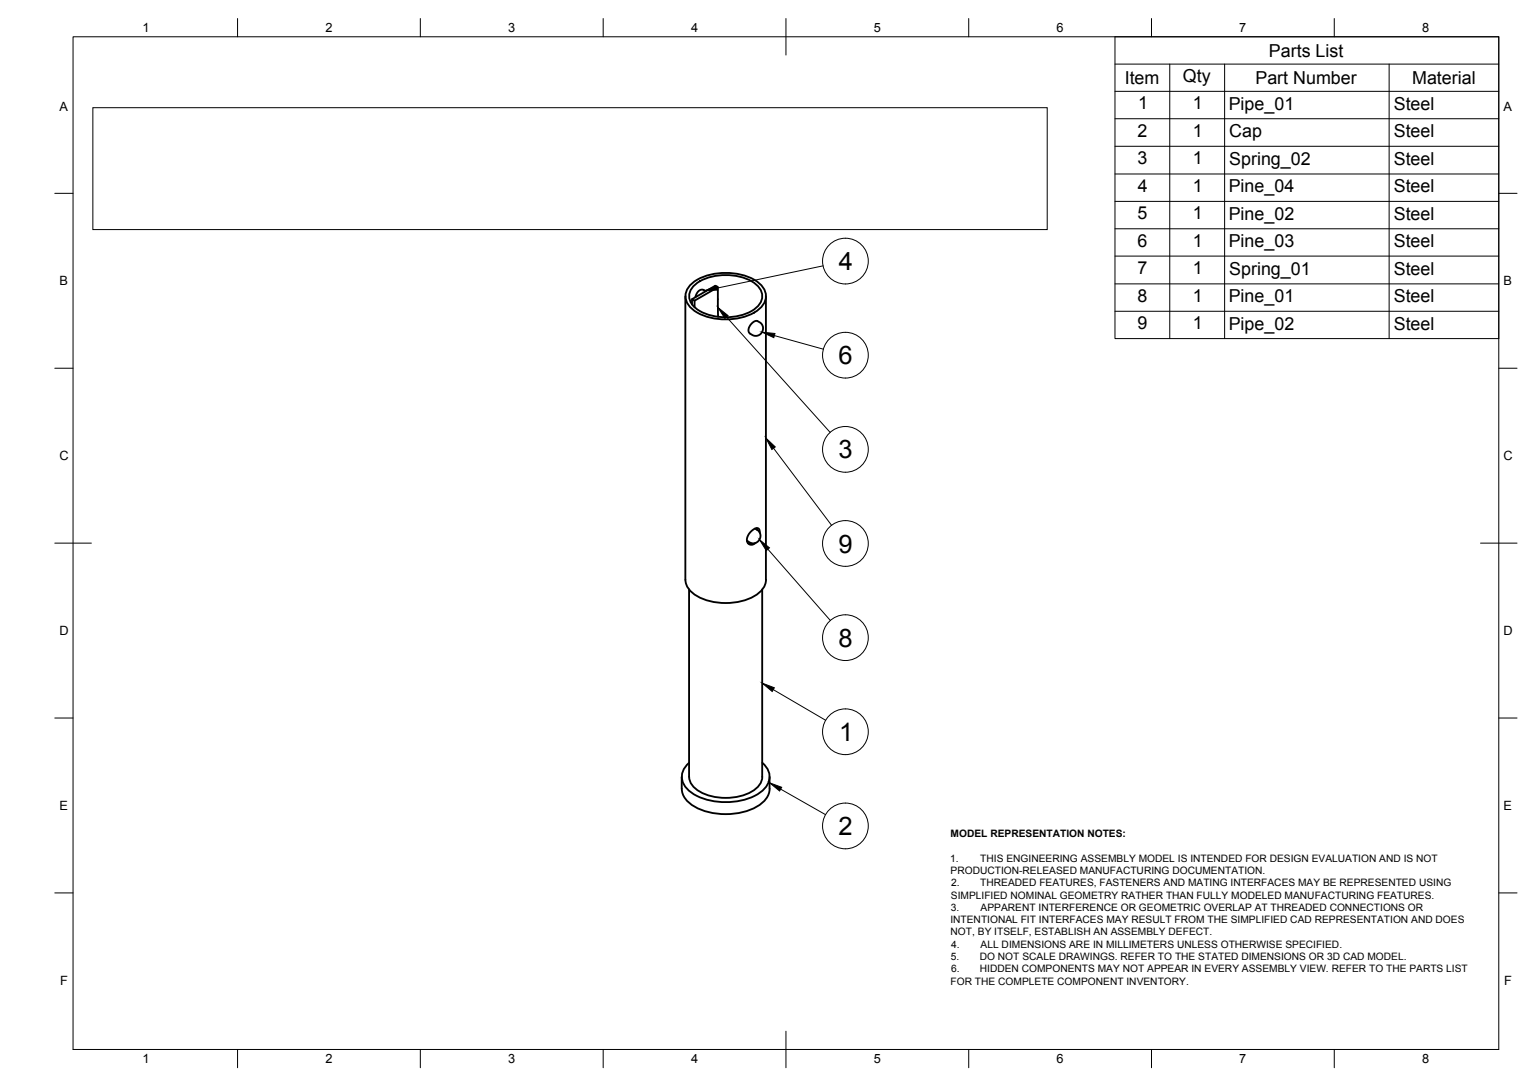
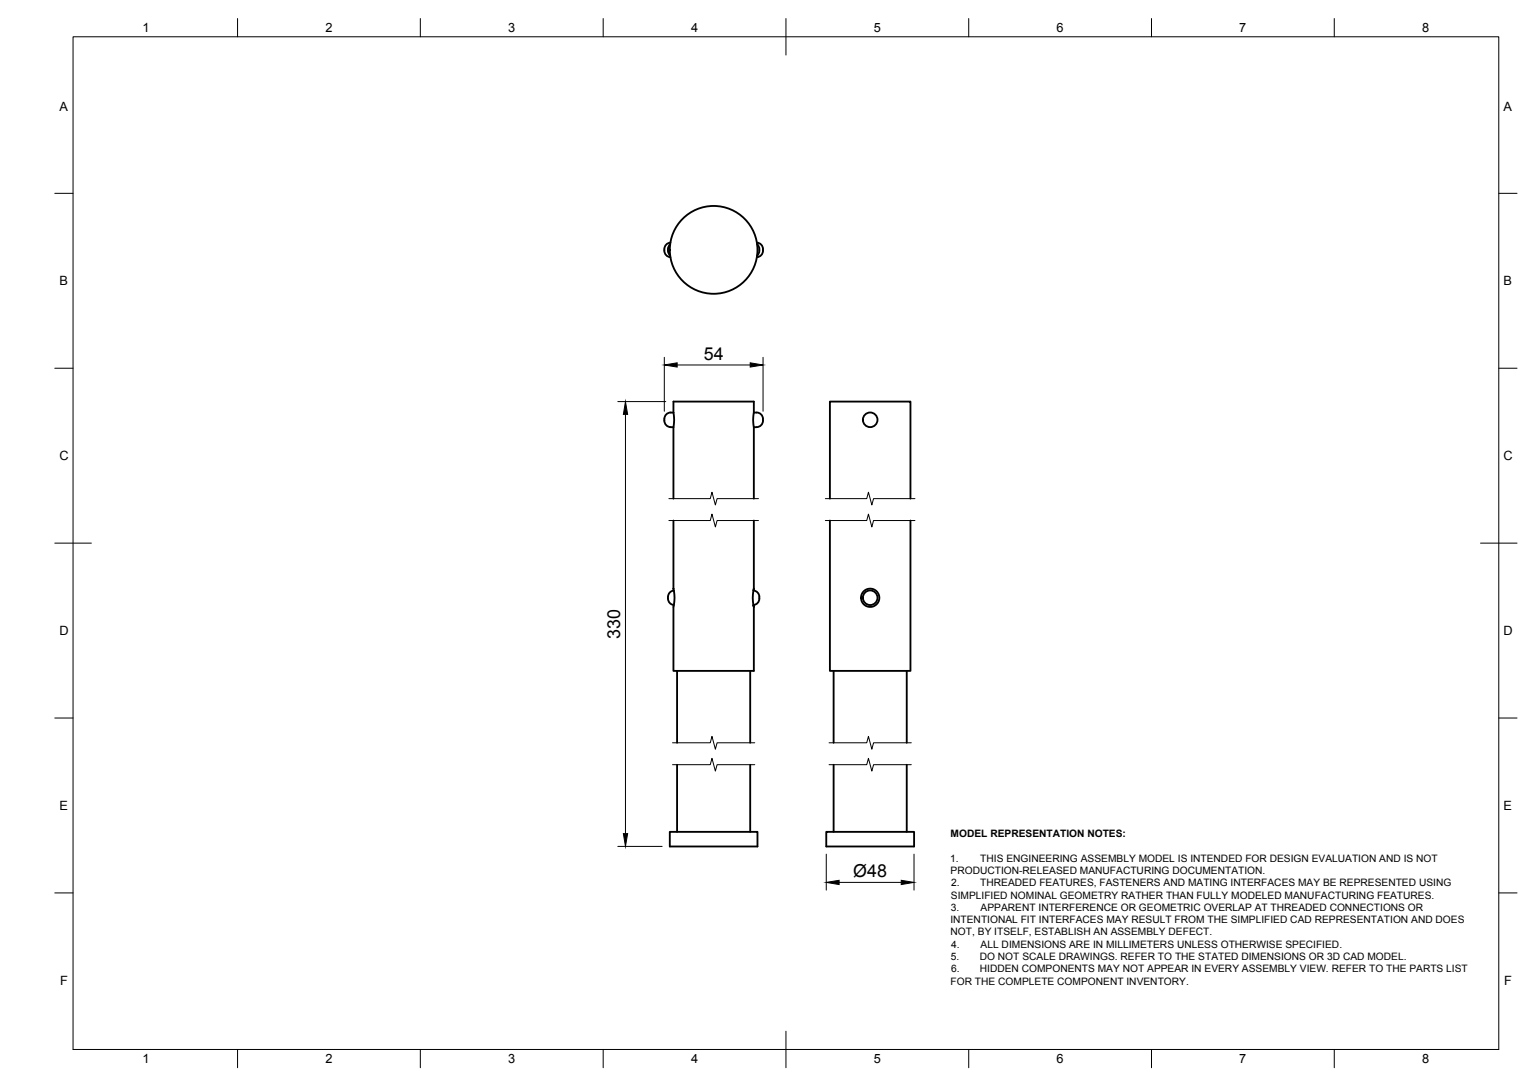
ISO-10303-21;
HEADER;
/* Generated by software containing ST-Developer
 * from STEP Tools, Inc. (www.steptools.com) 
 */

FILE_DESCRIPTION(
/* description */ (''),
/* implementation_level */ '2;1');

FILE_NAME(
/* name */ 'BR-354',
/* time_stamp */ '2026-10-06T13:31:15-07:00',
/* author */ (''),
/* organization */ (''),
/* preprocessor_version */ 'ST-DEVELOPER v20.2',
/* originating_system */ 'Autodesk Translation Framework v15.15.0.0',
/* authorisation */ '');

FILE_SCHEMA (('AUTOMOTIVE_DESIGN { 1 0 10303 214 3 1 1 }'));
ENDSEC;

DATA;
#10=MECHANICAL_DESIGN_GEOMETRIC_PRESENTATION_REPRESENTATION('',(#79,#80,
#81,#82,#83,#84,#85,#86,#87),#3154);
#11=ITEM_DEFINED_TRANSFORMATION($,$,#1191,#1277);
#12=ITEM_DEFINED_TRANSFORMATION($,$,#1202,#1278);
#13=ITEM_DEFINED_TRANSFORMATION($,$,#1212,#1279);
#14=ITEM_DEFINED_TRANSFORMATION($,$,#1221,#1280);
#15=ITEM_DEFINED_TRANSFORMATION($,$,#1230,#1281);
#16=ITEM_DEFINED_TRANSFORMATION($,$,#1239,#1282);
#17=ITEM_DEFINED_TRANSFORMATION($,$,#1248,#1283);
#18=ITEM_DEFINED_TRANSFORMATION($,$,#1257,#1284);
#19=ITEM_DEFINED_TRANSFORMATION($,$,#1266,#1285);
#20=(
REPRESENTATION_RELATIONSHIP($,$,#3189,#3188)
REPRESENTATION_RELATIONSHIP_WITH_TRANSFORMATION(#11)
SHAPE_REPRESENTATION_RELATIONSHIP()
);
#21=(
REPRESENTATION_RELATIONSHIP($,$,#3190,#3188)
REPRESENTATION_RELATIONSHIP_WITH_TRANSFORMATION(#12)
SHAPE_REPRESENTATION_RELATIONSHIP()
);
#22=(
REPRESENTATION_RELATIONSHIP($,$,#3191,#3188)
REPRESENTATION_RELATIONSHIP_WITH_TRANSFORMATION(#13)
SHAPE_REPRESENTATION_RELATIONSHIP()
);
#23=(
REPRESENTATION_RELATIONSHIP($,$,#3192,#3188)
REPRESENTATION_RELATIONSHIP_WITH_TRANSFORMATION(#14)
SHAPE_REPRESENTATION_RELATIONSHIP()
);
#24=(
REPRESENTATION_RELATIONSHIP($,$,#3193,#3188)
REPRESENTATION_RELATIONSHIP_WITH_TRANSFORMATION(#15)
SHAPE_REPRESENTATION_RELATIONSHIP()
);
#25=(
REPRESENTATION_RELATIONSHIP($,$,#3194,#3188)
REPRESENTATION_RELATIONSHIP_WITH_TRANSFORMATION(#16)
SHAPE_REPRESENTATION_RELATIONSHIP()
);
#26=(
REPRESENTATION_RELATIONSHIP($,$,#3195,#3188)
REPRESENTATION_RELATIONSHIP_WITH_TRANSFORMATION(#17)
SHAPE_REPRESENTATION_RELATIONSHIP()
);
#27=(
REPRESENTATION_RELATIONSHIP($,$,#3196,#3188)
REPRESENTATION_RELATIONSHIP_WITH_TRANSFORMATION(#18)
SHAPE_REPRESENTATION_RELATIONSHIP()
);
#28=(
REPRESENTATION_RELATIONSHIP($,$,#3197,#3188)
REPRESENTATION_RELATIONSHIP_WITH_TRANSFORMATION(#19)
SHAPE_REPRESENTATION_RELATIONSHIP()
);
#29=CONTEXT_DEPENDENT_SHAPE_REPRESENTATION(#20,#3179);
#30=CONTEXT_DEPENDENT_SHAPE_REPRESENTATION(#21,#3180);
#31=CONTEXT_DEPENDENT_SHAPE_REPRESENTATION(#22,#3181);
#32=CONTEXT_DEPENDENT_SHAPE_REPRESENTATION(#23,#3182);
#33=CONTEXT_DEPENDENT_SHAPE_REPRESENTATION(#24,#3183);
#34=CONTEXT_DEPENDENT_SHAPE_REPRESENTATION(#25,#3184);
#35=CONTEXT_DEPENDENT_SHAPE_REPRESENTATION(#26,#3185);
#36=CONTEXT_DEPENDENT_SHAPE_REPRESENTATION(#27,#3186);
#37=CONTEXT_DEPENDENT_SHAPE_REPRESENTATION(#28,#3187);
#38=NEXT_ASSEMBLY_USAGE_OCCURRENCE('Pipe_01:1','Pipe_01:1','Pipe_01:1',
#3199,#3200,'Pipe_01:1');
#39=NEXT_ASSEMBLY_USAGE_OCCURRENCE('Cap:1','Cap:1','Cap:1',#3199,#3201,
'Cap:1');
#40=NEXT_ASSEMBLY_USAGE_OCCURRENCE('Spring_02:1','Spring_02:1',
'Spring_02:1',#3199,#3202,'Spring_02:1');
#41=NEXT_ASSEMBLY_USAGE_OCCURRENCE('Pine_04:1','Pine_04:1','Pine_04:1',
#3199,#3203,'Pine_04:1');
#42=NEXT_ASSEMBLY_USAGE_OCCURRENCE('Pine_02:1','Pine_02:1','Pine_02:1',
#3199,#3204,'Pine_02:1');
#43=NEXT_ASSEMBLY_USAGE_OCCURRENCE('Pine_03:1','Pine_03:1','Pine_03:1',
#3199,#3205,'Pine_03:1');
#44=NEXT_ASSEMBLY_USAGE_OCCURRENCE('Spring_01:1','Spring_01:1',
'Spring_01:1',#3199,#3206,'Spring_01:1');
#45=NEXT_ASSEMBLY_USAGE_OCCURRENCE('Pine_01:1','Pine_01:1','Pine_01:1',
#3199,#3207,'Pine_01:1');
#46=NEXT_ASSEMBLY_USAGE_OCCURRENCE('Pipe_02:1','Pipe_02:1','Pipe_02:1',
#3199,#3208,'Pipe_02:1');
#47=(
BOUNDED_SURFACE()
B_SPLINE_SURFACE(2,2,((#2142,#2143,#2144,#2145,#2146,#2147,#2148,#2149,
#2150),(#2151,#2152,#2153,#2154,#2155,#2156,#2157,#2158,#2159),(#2160,#2161,
#2162,#2163,#2164,#2165,#2166,#2167,#2168)),.UNSPECIFIED.,.F.,.T.,.F.)
B_SPLINE_SURFACE_WITH_KNOTS((3,3),(3,2,2,2,3),(-1.57079632679497,6.11109985317371E-14),
(-3.14159265358979,-1.5707963267949,0.,1.5707963267949,3.14159265358979),
 .UNSPECIFIED.)
GEOMETRIC_REPRESENTATION_ITEM()
RATIONAL_B_SPLINE_SURFACE(((1.,0.707106781186548,1.,0.707106781186548,1.,
0.707106781186548,1.,0.707106781186548,1.),(0.707106781186505,0.49999999999997,
0.707106781186505,0.49999999999997,0.707106781186505,0.49999999999997,0.707106781186505,
0.49999999999997,0.707106781186505),(1.,0.707106781186548,1.,0.707106781186548,
1.,0.707106781186548,1.,0.707106781186548,1.)))
REPRESENTATION_ITEM('')
SURFACE()
);
#48=(
BOUNDED_SURFACE()
B_SPLINE_SURFACE(2,2,((#2183,#2184,#2185,#2186,#2187,#2188,#2189,#2190,
#2191),(#2192,#2193,#2194,#2195,#2196,#2197,#2198,#2199,#2200),(#2201,#2202,
#2203,#2204,#2205,#2206,#2207,#2208,#2209)),.UNSPECIFIED.,.F.,.T.,.F.)
B_SPLINE_SURFACE_WITH_KNOTS((3,3),(3,2,2,2,3),(-1.57079632679509,1.96675441490332E-13),
(-3.14159265358979,-1.5707963267949,0.,1.5707963267949,3.14159265358979),
 .UNSPECIFIED.)
GEOMETRIC_REPRESENTATION_ITEM()
RATIONAL_B_SPLINE_SURFACE(((1.,0.707106781186548,1.,0.707106781186548,1.,
0.707106781186548,1.,0.707106781186548,1.),(0.707106781186405,0.499999999999899,
0.707106781186405,0.499999999999899,0.707106781186405,0.499999999999899,
0.707106781186405,0.499999999999899,0.707106781186405),(1.,0.707106781186548,
1.,0.707106781186548,1.,0.707106781186548,1.,0.707106781186548,1.)))
REPRESENTATION_ITEM('')
SURFACE()
);
#49=(
BOUNDED_SURFACE()
B_SPLINE_SURFACE(2,2,((#2224,#2225,#2226,#2227,#2228,#2229,#2230,#2231,
#2232),(#2233,#2234,#2235,#2236,#2237,#2238,#2239,#2240,#2241),(#2242,#2243,
#2244,#2245,#2246,#2247,#2248,#2249,#2250)),.UNSPECIFIED.,.F.,.T.,.F.)
B_SPLINE_SURFACE_WITH_KNOTS((3,3),(3,2,2,2,3),(-6.11109985317371E-14,1.57079632679497),
(-3.14159265358979,-1.5707963267949,0.,1.5707963267949,3.14159265358979),
 .UNSPECIFIED.)
GEOMETRIC_REPRESENTATION_ITEM()
RATIONAL_B_SPLINE_SURFACE(((1.,0.707106781186548,1.,0.707106781186548,1.,
0.707106781186548,1.,0.707106781186548,1.),(0.707106781186505,0.49999999999997,
0.707106781186505,0.49999999999997,0.707106781186505,0.49999999999997,0.707106781186505,
0.49999999999997,0.707106781186505),(1.,0.707106781186548,1.,0.707106781186548,
1.,0.707106781186548,1.,0.707106781186548,1.)))
REPRESENTATION_ITEM('')
SURFACE()
);
#50=(
BOUNDED_SURFACE()
B_SPLINE_SURFACE(2,2,((#2568,#2569,#2570,#2571,#2572,#2573,#2574,#2575,
#2576),(#2577,#2578,#2579,#2580,#2581,#2582,#2583,#2584,#2585),(#2586,#2587,
#2588,#2589,#2590,#2591,#2592,#2593,#2594)),.UNSPECIFIED.,.F.,.T.,.F.)
B_SPLINE_SURFACE_WITH_KNOTS((3,3),(3,2,2,2,3),(-1.96675441490332E-13,1.57079632679509),
(-3.14159265358979,-1.5707963267949,0.,1.5707963267949,3.14159265358979),
 .UNSPECIFIED.)
GEOMETRIC_REPRESENTATION_ITEM()
RATIONAL_B_SPLINE_SURFACE(((1.,0.707106781186548,1.,0.707106781186548,1.,
0.707106781186548,1.,0.707106781186548,1.),(0.707106781186405,0.499999999999899,
0.707106781186405,0.499999999999899,0.707106781186405,0.499999999999899,
0.707106781186405,0.499999999999899,0.707106781186405),(1.,0.707106781186548,
1.,0.707106781186548,1.,0.707106781186548,1.,0.707106781186548,1.)))
REPRESENTATION_ITEM('')
SURFACE()
);
#51=B_SPLINE_SURFACE_WITH_KNOTS('',3,1,((#1764,#1765),(#1766,#1767),(#1768,
#1769),(#1770,#1771),(#1772,#1773),(#1774,#1775),(#1776,#1777),(#1778,#1779),
(#1780,#1781),(#1782,#1783),(#1784,#1785),(#1786,#1787),(#1788,#1789),(#1790,
#1791),(#1792,#1793),(#1794,#1795),(#1796,#1797),(#1798,#1799),(#1800,#1801)),
 .UNSPECIFIED.,.F.,.F.,.F.,(4,3,3,3,3,3,4),(2,2),(0.,0.25,0.625,0.869068416619454,
0.996324238316631,1.,1.10633190132162),(0.,2.16230058202055),
 .UNSPECIFIED.);
#52=B_SPLINE_SURFACE_WITH_KNOTS('',5,1,((#1843,#1844),(#1845,#1846),(#1847,
#1848),(#1849,#1850),(#1851,#1852),(#1853,#1854),(#1855,#1856),(#1857,#1858),
(#1859,#1860),(#1861,#1862),(#1863,#1864),(#1865,#1866),(#1867,#1868),(#1869,
#1870),(#1871,#1872),(#1873,#1874),(#1875,#1876),(#1877,#1878),(#1879,#1880),
(#1881,#1882),(#1883,#1884),(#1885,#1886),(#1887,#1888),(#1889,#1890),(#1891,
#1892)),.UNSPECIFIED.,.F.,.F.,.F.,(6,5,1,1,1,1,1,1,1,1,1,1,1,1,1,1,6),(2,
2),(-1.10044937423827,-1.,-0.933333333333333,-0.866666666666667,-0.8,-0.733333333333333,
-0.666666666666667,-0.6,-0.533333333333333,-0.466666666666667,-0.4,-0.333333333333333,
-0.266666666666667,-0.2,-0.133333333333333,-0.0666666666666667,0.),(0.,
2.16),.UNSPECIFIED.);
#53=B_SPLINE_SURFACE_WITH_KNOTS('',5,1,((#2046,#2047),(#2048,#2049),(#2050,
#2051),(#2052,#2053),(#2054,#2055),(#2056,#2057),(#2058,#2059),(#2060,#2061),
(#2062,#2063),(#2064,#2065),(#2066,#2067),(#2068,#2069),(#2070,#2071),(#2072,
#2073),(#2074,#2075),(#2076,#2077),(#2078,#2079),(#2080,#2081),(#2082,#2083),
(#2084,#2085),(#2086,#2087),(#2088,#2089),(#2090,#2091),(#2092,#2093),(#2094,
#2095)),.UNSPECIFIED.,.F.,.F.,.F.,(6,1,1,1,1,1,1,1,1,1,1,1,1,1,1,5,6),(2,
2),(0.,0.0666666666666667,0.133333333333333,0.2,0.266666666666667,0.333333333333333,
0.4,0.466666666666667,0.533333333333333,0.6,0.666666666666667,0.733333333333333,
0.8,0.866666666666667,0.933333333333333,1.,1.10044937423827),(0.,2.16),
 .UNSPECIFIED.);
#54=B_SPLINE_SURFACE_WITH_KNOTS('',3,1,((#2103,#2104),(#2105,#2106),(#2107,
#2108),(#2109,#2110),(#2111,#2112),(#2113,#2114),(#2115,#2116),(#2117,#2118),
(#2119,#2120),(#2121,#2122),(#2123,#2124),(#2125,#2126),(#2127,#2128),(#2129,
#2130),(#2131,#2132),(#2133,#2134),(#2135,#2136),(#2137,#2138),(#2139,#2140)),
 .UNSPECIFIED.,.F.,.F.,.F.,(4,3,3,3,3,3,4),(2,2),(-1.10633190132173,-1.,
-0.996324238316733,-0.869068416619454,-0.625,-0.25,0.),(0.,2.16230058202055),
 .UNSPECIFIED.);
#55=B_SPLINE_SURFACE_WITH_KNOTS('',5,1,((#2342,#2343),(#2344,#2345),(#2346,
#2347),(#2348,#2349),(#2350,#2351),(#2352,#2353),(#2354,#2355),(#2356,#2357),
(#2358,#2359),(#2360,#2361),(#2362,#2363),(#2364,#2365),(#2366,#2367),(#2368,
#2369),(#2370,#2371),(#2372,#2373),(#2374,#2375),(#2376,#2377),(#2378,#2379),
(#2380,#2381)),.UNSPECIFIED.,.F.,.F.,.F.,(6,1,1,1,1,1,1,1,1,1,1,1,1,1,1,
6),(2,2),(-1.,-0.933333333333333,-0.866666666666667,-0.8,-0.733333333333333,
-0.666666666666667,-0.6,-0.533333333333333,-0.466666666666667,-0.4,-0.333333333333333,
-0.266666666666667,-0.2,-0.133333333333333,-0.0666666666666667,0.),(0.,
2.16),.UNSPECIFIED.);
#56=B_SPLINE_SURFACE_WITH_KNOTS('',5,1,((#2406,#2407),(#2408,#2409),(#2410,
#2411),(#2412,#2413),(#2414,#2415),(#2416,#2417),(#2418,#2419),(#2420,#2421),
(#2422,#2423),(#2424,#2425),(#2426,#2427),(#2428,#2429),(#2430,#2431),(#2432,
#2433),(#2434,#2435),(#2436,#2437),(#2438,#2439),(#2440,#2441),(#2442,#2443),
(#2444,#2445)),.UNSPECIFIED.,.F.,.F.,.F.,(6,1,1,1,1,1,1,1,1,1,1,1,1,1,1,
6),(2,2),(0.,0.0666666666666667,0.133333333333333,0.2,0.266666666666667,
0.333333333333333,0.4,0.466666666666667,0.533333333333333,0.6,0.666666666666667,
0.733333333333333,0.8,0.866666666666667,0.933333333333333,1.),(0.,2.16),
 .UNSPECIFIED.);
#57=B_SPLINE_SURFACE_WITH_KNOTS('',3,1,((#2480,#2481),(#2482,#2483),(#2484,
#2485),(#2486,#2487),(#2488,#2489),(#2490,#2491),(#2492,#2493),(#2494,#2495),
(#2496,#2497),(#2498,#2499),(#2500,#2501),(#2502,#2503),(#2504,#2505)),
 .UNSPECIFIED.,.F.,.F.,.F.,(4,3,3,3,4),(2,2),(-0.996324238316733,-0.869068416619454,
-0.625,-0.25,0.),(0.,2.16230058202055),.UNSPECIFIED.);
#58=B_SPLINE_SURFACE_WITH_KNOTS('',3,1,((#2518,#2519),(#2520,#2521),(#2522,
#2523),(#2524,#2525),(#2526,#2527),(#2528,#2529),(#2530,#2531),(#2532,#2533),
(#2534,#2535),(#2536,#2537),(#2538,#2539),(#2540,#2541),(#2542,#2543)),
 .UNSPECIFIED.,.F.,.F.,.F.,(4,3,3,3,4),(2,2),(0.,0.25,0.625,0.869068416619454,
0.996324238316631),(0.,2.16230058202055),.UNSPECIFIED.);
#59=B_SPLINE_SURFACE_WITH_KNOTS('',3,1,((#2777,#2778),(#2779,#2780),(#2781,
#2782),(#2783,#2784),(#2785,#2786),(#2787,#2788),(#2789,#2790),(#2791,#2792),
(#2793,#2794),(#2795,#2796),(#2797,#2798),(#2799,#2800),(#2801,#2802),(#2803,
#2804),(#2805,#2806),(#2807,#2808),(#2809,#2810),(#2811,#2812),(#2813,#2814),
(#2815,#2816),(#2817,#2818),(#2819,#2820),(#2821,#2822),(#2823,#2824),(#2825,
#2826),(#2827,#2828),(#2829,#2830),(#2831,#2832),(#2833,#2834),(#2835,#2836),
(#2837,#2838),(#2839,#2840),(#2841,#2842),(#2843,#2844),(#2845,#2846),(#2847,
#2848),(#2849,#2850)),.UNSPECIFIED.,.T.,.F.,.F.,(4,3,3,3,3,3,3,3,3,3,3,
3,4),(2,2),(-2.41782189489405,-2.24947880033894,-1.98878599548315,-1.8058107663078,
-1.62285095130575,-1.4611068129162,-1.2281083508595,-1.04723806876992,-0.775359720885815,
-0.597430394095587,-0.415845402852008,-0.241029560217643,0.),(0.,28.8022414300165),
 .UNSPECIFIED.);
#60=B_SPLINE_SURFACE_WITH_KNOTS('',3,1,((#2932,#2933),(#2934,#2935),(#2936,
#2937),(#2938,#2939),(#2940,#2941),(#2942,#2943),(#2944,#2945),(#2946,#2947),
(#2948,#2949),(#2950,#2951),(#2952,#2953),(#2954,#2955),(#2956,#2957),(#2958,
#2959),(#2960,#2961),(#2962,#2963),(#2964,#2965),(#2966,#2967),(#2968,#2969),
(#2970,#2971),(#2972,#2973),(#2974,#2975),(#2976,#2977),(#2978,#2979),(#2980,
#2981),(#2982,#2983),(#2984,#2985),(#2986,#2987),(#2988,#2989),(#2990,#2991),
(#2992,#2993),(#2994,#2995),(#2996,#2997),(#2998,#2999),(#3000,#3001),(#3002,
#3003),(#3004,#3005)),.UNSPECIFIED.,.T.,.F.,.F.,(4,3,3,3,3,3,3,3,3,3,3,
3,4),(2,2),(-2.41782189489405,-2.24947880033894,-1.98878599548315,-1.8058107663078,
-1.62285095130575,-1.4611068129162,-1.2281083508595,-1.04723806876992,-0.775359720885815,
-0.597430394095587,-0.415845402852008,-0.241029560217643,0.),(0.,28.8022414300165),
 .UNSPECIFIED.);
#61=SHAPE_REPRESENTATION_RELATIONSHIP('SRR','None',#3189,#70);
#62=SHAPE_REPRESENTATION_RELATIONSHIP('SRR','None',#3190,#71);
#63=SHAPE_REPRESENTATION_RELATIONSHIP('SRR','None',#3191,#72);
#64=SHAPE_REPRESENTATION_RELATIONSHIP('SRR','None',#3192,#73);
#65=SHAPE_REPRESENTATION_RELATIONSHIP('SRR','None',#3193,#74);
#66=SHAPE_REPRESENTATION_RELATIONSHIP('SRR','None',#3194,#75);
#67=SHAPE_REPRESENTATION_RELATIONSHIP('SRR','None',#3195,#76);
#68=SHAPE_REPRESENTATION_RELATIONSHIP('SRR','None',#3196,#77);
#69=SHAPE_REPRESENTATION_RELATIONSHIP('SRR','None',#3197,#78);
#70=ADVANCED_BREP_SHAPE_REPRESENTATION('',(#88),#3145);
#71=ADVANCED_BREP_SHAPE_REPRESENTATION('',(#89),#3146);
#72=ADVANCED_BREP_SHAPE_REPRESENTATION('',(#90),#3147);
#73=ADVANCED_BREP_SHAPE_REPRESENTATION('',(#91),#3148);
#74=ADVANCED_BREP_SHAPE_REPRESENTATION('',(#92),#3149);
#75=ADVANCED_BREP_SHAPE_REPRESENTATION('',(#93),#3150);
#76=ADVANCED_BREP_SHAPE_REPRESENTATION('',(#94),#3151);
#77=ADVANCED_BREP_SHAPE_REPRESENTATION('',(#95),#3152);
#78=ADVANCED_BREP_SHAPE_REPRESENTATION('',(#96),#3153);
#79=STYLED_ITEM('',(#3243),#88);
#80=STYLED_ITEM('',(#3243),#89);
#81=STYLED_ITEM('',(#3243),#90);
#82=STYLED_ITEM('',(#3243),#91);
#83=STYLED_ITEM('',(#3243),#92);
#84=STYLED_ITEM('',(#3243),#93);
#85=STYLED_ITEM('',(#3243),#94);
#86=STYLED_ITEM('',(#3243),#95);
#87=STYLED_ITEM('',(#3243),#96);
#88=MANIFOLD_SOLID_BREP('Body1',#1081);
#89=MANIFOLD_SOLID_BREP('Body1',#1082);
#90=MANIFOLD_SOLID_BREP('Body1',#1083);
#91=MANIFOLD_SOLID_BREP('Body1',#1084);
#92=MANIFOLD_SOLID_BREP('Body1',#1085);
#93=MANIFOLD_SOLID_BREP('Body1',#1086);
#94=MANIFOLD_SOLID_BREP('Body1',#1087);
#95=MANIFOLD_SOLID_BREP('Body1',#1088);
#96=MANIFOLD_SOLID_BREP('Body1',#1089);
#97=PLANE('',#1200);
#98=PLANE('',#1201);
#99=PLANE('',#1203);
#100=PLANE('',#1210);
#101=PLANE('',#1211);
#102=PLANE('',#1213);
#103=PLANE('',#1214);
#104=PLANE('',#1215);
#105=PLANE('',#1216);
#106=PLANE('',#1217);
#107=PLANE('',#1218);
#108=PLANE('',#1219);
#109=PLANE('',#1220);
#110=PLANE('',#1228);
#111=PLANE('',#1229);
#112=PLANE('',#1237);
#113=PLANE('',#1238);
#114=PLANE('',#1246);
#115=PLANE('',#1247);
#116=PLANE('',#1249);
#117=PLANE('',#1250);
#118=PLANE('',#1251);
#119=PLANE('',#1252);
#120=PLANE('',#1253);
#121=PLANE('',#1254);
#122=PLANE('',#1255);
#123=PLANE('',#1256);
#124=PLANE('',#1264);
#125=PLANE('',#1265);
#126=PLANE('',#1269);
#127=PLANE('',#1276);
#128=FACE_BOUND('',#233,.T.);
#129=FACE_BOUND('',#235,.T.);
#130=FACE_BOUND('',#237,.T.);
#131=FACE_BOUND('',#239,.T.);
#132=FACE_BOUND('',#245,.T.);
#133=FACE_BOUND('',#291,.T.);
#134=FACE_BOUND('',#293,.T.);
#135=FACE_BOUND('',#294,.T.);
#136=FACE_BOUND('',#296,.T.);
#137=FACE_BOUND('',#297,.T.);
#138=FACE_BOUND('',#299,.T.);
#139=CIRCLE('',#1195,18.);
#140=CIRCLE('',#1196,18.);
#141=CIRCLE('',#1198,20.);
#142=CIRCLE('',#1199,20.);
#143=CIRCLE('',#1204,20.);
#144=CIRCLE('',#1206,20.);
#145=CIRCLE('',#1208,24.);
#146=CIRCLE('',#1209,24.);
#147=CIRCLE('',#1222,3.99999999999999);
#148=CIRCLE('',#1223,3.99999999999999);
#149=CIRCLE('',#1224,3.49999999999999);
#150=CIRCLE('',#1225,0.49999999999999);
#151=CIRCLE('',#1227,3.99999999999999);
#152=CIRCLE('',#1231,3.99999999999999);
#153=CIRCLE('',#1232,3.99999999999999);
#154=CIRCLE('',#1233,3.49999999999994);
#155=CIRCLE('',#1234,0.49999999999999);
#156=CIRCLE('',#1236,3.99999999999999);
#157=CIRCLE('',#1240,3.99999999999999);
#158=CIRCLE('',#1241,3.49999999999999);
#159=CIRCLE('',#1242,0.49999999999999);
#160=CIRCLE('',#1243,3.99999999999999);
#161=CIRCLE('',#1245,3.99999999999999);
#162=CIRCLE('',#1258,3.99999999999999);
#163=CIRCLE('',#1259,3.49999999999994);
#164=CIRCLE('',#1260,0.49999999999999);
#165=CIRCLE('',#1261,3.99999999999999);
#166=CIRCLE('',#1263,3.99999999999999);
#167=CIRCLE('',#1270,22.);
#168=CIRCLE('',#1271,20.);
#169=CIRCLE('',#1273,20.);
#170=CIRCLE('',#1275,22.);
#171=FACE_OUTER_BOUND('',#230,.T.);
#172=FACE_OUTER_BOUND('',#231,.T.);
#173=FACE_OUTER_BOUND('',#232,.T.);
#174=FACE_OUTER_BOUND('',#234,.T.);
#175=FACE_OUTER_BOUND('',#236,.T.);
#176=FACE_OUTER_BOUND('',#238,.T.);
#177=FACE_OUTER_BOUND('',#240,.T.);
#178=FACE_OUTER_BOUND('',#241,.T.);
#179=FACE_OUTER_BOUND('',#242,.T.);
#180=FACE_OUTER_BOUND('',#243,.T.);
#181=FACE_OUTER_BOUND('',#244,.T.);
#182=FACE_OUTER_BOUND('',#246,.T.);
#183=FACE_OUTER_BOUND('',#247,.T.);
#184=FACE_OUTER_BOUND('',#248,.T.);
#185=FACE_OUTER_BOUND('',#249,.T.);
#186=FACE_OUTER_BOUND('',#250,.T.);
#187=FACE_OUTER_BOUND('',#251,.T.);
#188=FACE_OUTER_BOUND('',#252,.T.);
#189=FACE_OUTER_BOUND('',#253,.T.);
#190=FACE_OUTER_BOUND('',#254,.T.);
#191=FACE_OUTER_BOUND('',#255,.T.);
#192=FACE_OUTER_BOUND('',#256,.T.);
#193=FACE_OUTER_BOUND('',#257,.T.);
#194=FACE_OUTER_BOUND('',#258,.T.);
#195=FACE_OUTER_BOUND('',#259,.T.);
#196=FACE_OUTER_BOUND('',#260,.T.);
#197=FACE_OUTER_BOUND('',#261,.T.);
#198=FACE_OUTER_BOUND('',#262,.T.);
#199=FACE_OUTER_BOUND('',#263,.T.);
#200=FACE_OUTER_BOUND('',#264,.T.);
#201=FACE_OUTER_BOUND('',#265,.T.);
#202=FACE_OUTER_BOUND('',#266,.T.);
#203=FACE_OUTER_BOUND('',#267,.T.);
#204=FACE_OUTER_BOUND('',#268,.T.);
#205=FACE_OUTER_BOUND('',#269,.T.);
#206=FACE_OUTER_BOUND('',#270,.T.);
#207=FACE_OUTER_BOUND('',#271,.T.);
#208=FACE_OUTER_BOUND('',#272,.T.);
#209=FACE_OUTER_BOUND('',#273,.T.);
#210=FACE_OUTER_BOUND('',#274,.T.);
#211=FACE_OUTER_BOUND('',#275,.T.);
#212=FACE_OUTER_BOUND('',#276,.T.);
#213=FACE_OUTER_BOUND('',#277,.T.);
#214=FACE_OUTER_BOUND('',#278,.T.);
#215=FACE_OUTER_BOUND('',#279,.T.);
#216=FACE_OUTER_BOUND('',#280,.T.);
#217=FACE_OUTER_BOUND('',#281,.T.);
#218=FACE_OUTER_BOUND('',#282,.T.);
#219=FACE_OUTER_BOUND('',#283,.T.);
#220=FACE_OUTER_BOUND('',#284,.T.);
#221=FACE_OUTER_BOUND('',#285,.T.);
#222=FACE_OUTER_BOUND('',#286,.T.);
#223=FACE_OUTER_BOUND('',#287,.T.);
#224=FACE_OUTER_BOUND('',#288,.T.);
#225=FACE_OUTER_BOUND('',#289,.T.);
#226=FACE_OUTER_BOUND('',#290,.T.);
#227=FACE_OUTER_BOUND('',#292,.T.);
#228=FACE_OUTER_BOUND('',#295,.T.);
#229=FACE_OUTER_BOUND('',#298,.T.);
#230=EDGE_LOOP('',(#720,#721,#722,#723,#724,#725,#726,#727));
#231=EDGE_LOOP('',(#728,#729,#730,#731,#732,#733));
#232=EDGE_LOOP('',(#734,#735,#736,#737,#738,#739,#740,#741,#742));
#233=EDGE_LOOP('',(#743,#744));
#234=EDGE_LOOP('',(#745,#746,#747,#748,#749,#750,#751,#752,#753));
#235=EDGE_LOOP('',(#754,#755));
#236=EDGE_LOOP('',(#756));
#237=EDGE_LOOP('',(#757));
#238=EDGE_LOOP('',(#758));
#239=EDGE_LOOP('',(#759));
#240=EDGE_LOOP('',(#760));
#241=EDGE_LOOP('',(#761,#762,#763,#764));
#242=EDGE_LOOP('',(#765,#766,#767,#768));
#243=EDGE_LOOP('',(#769));
#244=EDGE_LOOP('',(#770));
#245=EDGE_LOOP('',(#771));
#246=EDGE_LOOP('',(#772,#773,#774,#775));
#247=EDGE_LOOP('',(#776,#777,#778,#779));
#248=EDGE_LOOP('',(#780,#781,#782,#783));
#249=EDGE_LOOP('',(#784,#785,#786,#787));
#250=EDGE_LOOP('',(#788,#789,#790,#791));
#251=EDGE_LOOP('',(#792,#793,#794,#795,#796,#797,#798,#799,#800,#801));
#252=EDGE_LOOP('',(#802,#803,#804,#805,#806,#807,#808,#809,#810,#811));
#253=EDGE_LOOP('',(#812,#813,#814,#815));
#254=EDGE_LOOP('',(#816,#817,#818,#819));
#255=EDGE_LOOP('',(#820,#821,#822,#823));
#256=EDGE_LOOP('',(#824,#825,#826,#827));
#257=EDGE_LOOP('',(#828,#829,#830,#831));
#258=EDGE_LOOP('',(#832,#833,#834,#835,#836));
#259=EDGE_LOOP('',(#837,#838,#839,#840,#841));
#260=EDGE_LOOP('',(#842));
#261=EDGE_LOOP('',(#843));
#262=EDGE_LOOP('',(#844,#845,#846,#847,#848));
#263=EDGE_LOOP('',(#849,#850,#851,#852,#853));
#264=EDGE_LOOP('',(#854));
#265=EDGE_LOOP('',(#855));
#266=EDGE_LOOP('',(#856,#857,#858,#859,#860));
#267=EDGE_LOOP('',(#861,#862,#863,#864,#865));
#268=EDGE_LOOP('',(#866));
#269=EDGE_LOOP('',(#867));
#270=EDGE_LOOP('',(#868,#869,#870,#871,#872,#873,#874,#875,#876,#877));
#271=EDGE_LOOP('',(#878,#879,#880,#881));
#272=EDGE_LOOP('',(#882,#883,#884,#885));
#273=EDGE_LOOP('',(#886,#887,#888,#889));
#274=EDGE_LOOP('',(#890,#891,#892,#893));
#275=EDGE_LOOP('',(#894,#895,#896,#897));
#276=EDGE_LOOP('',(#898,#899,#900,#901));
#277=EDGE_LOOP('',(#902,#903,#904,#905));
#278=EDGE_LOOP('',(#906,#907,#908,#909));
#279=EDGE_LOOP('',(#910,#911,#912,#913));
#280=EDGE_LOOP('',(#914,#915,#916,#917));
#281=EDGE_LOOP('',(#918,#919,#920,#921,#922,#923,#924,#925,#926,#927));
#282=EDGE_LOOP('',(#928,#929,#930,#931,#932));
#283=EDGE_LOOP('',(#933,#934,#935,#936,#937));
#284=EDGE_LOOP('',(#938));
#285=EDGE_LOOP('',(#939));
#286=EDGE_LOOP('',(#940,#941,#942,#943,#944,#945));
#287=EDGE_LOOP('',(#946,#947,#948,#949,#950,#951,#952,#953,#954,#955));
#288=EDGE_LOOP('',(#956,#957,#958,#959));
#289=EDGE_LOOP('',(#960,#961,#962,#963,#964,#965,#966,#967));
#290=EDGE_LOOP('',(#968));
#291=EDGE_LOOP('',(#969));
#292=EDGE_LOOP('',(#970,#971,#972,#973,#974,#975,#976,#977,#978,#979,#980,
#981,#982,#983,#984));
#293=EDGE_LOOP('',(#985,#986));
#294=EDGE_LOOP('',(#987));
#295=EDGE_LOOP('',(#988,#989,#990,#991,#992,#993,#994,#995,#996,#997,#998,
#999,#1000,#1001,#1002));
#296=EDGE_LOOP('',(#1003,#1004));
#297=EDGE_LOOP('',(#1005));
#298=EDGE_LOOP('',(#1006));
#299=EDGE_LOOP('',(#1007));
#300=LINE('',#1580,#366);
#301=LINE('',#1672,#367);
#302=LINE('',#1713,#368);
#303=LINE('',#1715,#369);
#304=LINE('',#1720,#370);
#305=LINE('',#1722,#371);
#306=LINE('',#1732,#372);
#307=LINE('',#1738,#373);
#308=LINE('',#1746,#374);
#309=LINE('',#1748,#375);
#310=LINE('',#1750,#376);
#311=LINE('',#1751,#377);
#312=LINE('',#1755,#378);
#313=LINE('',#1756,#379);
#314=LINE('',#1757,#380);
#315=LINE('',#1761,#381);
#316=LINE('',#1762,#382);
#317=LINE('',#1763,#383);
#318=LINE('',#1804,#384);
#319=LINE('',#1919,#385);
#320=LINE('',#1966,#386);
#321=LINE('',#1968,#387);
#322=LINE('',#1970,#388);
#323=LINE('',#2022,#389);
#324=LINE('',#2024,#390);
#325=LINE('',#2026,#391);
#326=LINE('',#2096,#392);
#327=LINE('',#2098,#393);
#328=LINE('',#2100,#394);
#329=LINE('',#2102,#395);
#330=LINE('',#2179,#396);
#331=LINE('',#2220,#397);
#332=LINE('',#2260,#398);
#333=LINE('',#2268,#399);
#334=LINE('',#2312,#400);
#335=LINE('',#2314,#401);
#336=LINE('',#2316,#402);
#337=LINE('',#2340,#403);
#338=LINE('',#2341,#404);
#339=LINE('',#2383,#405);
#340=LINE('',#2405,#406);
#341=LINE('',#2467,#407);
#342=LINE('',#2470,#408);
#343=LINE('',#2471,#409);
#344=LINE('',#2474,#410);
#345=LINE('',#2475,#411);
#346=LINE('',#2478,#412);
#347=LINE('',#2479,#413);
#348=LINE('',#2517,#414);
#349=LINE('',#2555,#415);
#350=LINE('',#2558,#416);
#351=LINE('',#2559,#417);
#352=LINE('',#2562,#418);
#353=LINE('',#2563,#419);
#354=LINE('',#2565,#420);
#355=LINE('',#2604,#421);
#356=LINE('',#2649,#422);
#357=LINE('',#2723,#423);
#358=LINE('',#2892,#424);
#359=LINE('',#3023,#425);
#360=LINE('',#3112,#426);
#361=LINE('',#3113,#427);
#362=LINE('',#3115,#428);
#363=LINE('',#3120,#429);
#364=LINE('',#3121,#430);
#365=LINE('',#3122,#431);
#366=VECTOR('',#1292,3.99999999999999);
#367=VECTOR('',#1295,3.99999999999999);
#368=VECTOR('',#1300,18.);
#369=VECTOR('',#1301,18.);
#370=VECTOR('',#1308,20.);
#371=VECTOR('',#1309,20.);
#372=VECTOR('',#1324,20.);
#373=VECTOR('',#1331,24.);
#374=VECTOR('',#1342,10.);
#375=VECTOR('',#1343,10.);
#376=VECTOR('',#1344,10.);
#377=VECTOR('',#1345,10.);
#378=VECTOR('',#1348,10.);
#379=VECTOR('',#1349,10.);
#380=VECTOR('',#1350,10.);
#381=VECTOR('',#1353,10.);
#382=VECTOR('',#1354,10.);
#383=VECTOR('',#1355,10.);
#384=VECTOR('',#1356,10.);
#385=VECTOR('',#1357,10.);
#386=VECTOR('',#1360,10.);
#387=VECTOR('',#1361,10.);
#388=VECTOR('',#1362,10.);
#389=VECTOR('',#1365,10.);
#390=VECTOR('',#1366,10.);
#391=VECTOR('',#1367,10.);
#392=VECTOR('',#1368,10.);
#393=VECTOR('',#1371,10.);
#394=VECTOR('',#1374,10.);
#395=VECTOR('',#1377,10.);
#396=VECTOR('',#1392,3.99999999999999);
#397=VECTOR('',#1411,3.99999999999999);
#398=VECTOR('',#1428,3.99999999999999);
#399=VECTOR('',#1439,10.);
#400=VECTOR('',#1440,10.);
#401=VECTOR('',#1441,10.);
#402=VECTOR('',#1442,10.);
#403=VECTOR('',#1443,10.);
#404=VECTOR('',#1444,10.);
#405=VECTOR('',#1445,10.);
#406=VECTOR('',#1446,10.);
#407=VECTOR('',#1447,10.);
#408=VECTOR('',#1450,10.);
#409=VECTOR('',#1451,10.);
#410=VECTOR('',#1454,10.);
#411=VECTOR('',#1455,10.);
#412=VECTOR('',#1458,10.);
#413=VECTOR('',#1459,10.);
#414=VECTOR('',#1460,10.);
#415=VECTOR('',#1461,10.);
#416=VECTOR('',#1464,10.);
#417=VECTOR('',#1465,10.);
#418=VECTOR('',#1468,10.);
#419=VECTOR('',#1469,10.);
#420=VECTOR('',#1472,10.);
#421=VECTOR('',#1487,3.99999999999999);
#422=VECTOR('',#1498,3.99999999999999);
#423=VECTOR('',#1501,3.99999999999999);
#424=VECTOR('',#1502,10.);
#425=VECTOR('',#1503,10.);
#426=VECTOR('',#1512,20.);
#427=VECTOR('',#1513,20.);
#428=VECTOR('',#1514,20.);
#429=VECTOR('',#1521,22.);
#430=VECTOR('',#1522,22.);
#431=VECTOR('',#1523,22.);
#432=B_SPLINE_CURVE_WITH_KNOTS('',3,(#1549,#1550,#1551,#1552,#1553,#1554,
#1555,#1556,#1557,#1558,#1559,#1560,#1561,#1562,#1563,#1564,#1565,#1566,
#1567),.UNSPECIFIED.,.F.,.F.,(4,2,2,2,3,2,2,2,4),(-0.604455473723513,-0.453345839217834,
-0.302236204712155,-0.151118102356077,0.,0.151118102356077,0.302236204712155,
0.453345839217834,0.604455473723513),.UNSPECIFIED.);
#433=B_SPLINE_CURVE_WITH_KNOTS('',3,(#1569,#1570,#1571,#1572,#1573,#1574,
#1575,#1576,#1577,#1578),.UNSPECIFIED.,.F.,.F.,(4,2,2,2,4),(-1.81336642117054,
-1.66225678666486,-1.51114715215918,-1.3600290498031,-1.20891094744703),
 .UNSPECIFIED.);
#434=B_SPLINE_CURVE_WITH_KNOTS('',3,(#1582,#1583,#1584,#1585,#1586,#1587,
#1588,#1589,#1590,#1591),.UNSPECIFIED.,.F.,.F.,(4,2,2,2,4),(1.20975547030872,
1.36098142054494,1.51220737078115,1.66342028812212,1.81463320546308),
 .UNSPECIFIED.);
#435=B_SPLINE_CURVE_WITH_KNOTS('',3,(#1593,#1594,#1595,#1596,#1597,#1598,
#1599,#1600,#1601,#1602,#1603,#1604,#1605,#1606,#1607,#1608,#1609,#1610,
#1611),.UNSPECIFIED.,.F.,.F.,(4,2,2,2,3,2,2,2,4),(1.81463320546308,1.96584612280404,
2.11705904014501,2.26828499038122,2.41951094061744,2.57073689085366,2.72196284108987,
2.87317575843084,3.0243886757718),.UNSPECIFIED.);
#436=B_SPLINE_CURVE_WITH_KNOTS('',3,(#1612,#1613,#1614,#1615,#1616,#1617,
#1618,#1619,#1620,#1621),.UNSPECIFIED.,.F.,.F.,(4,2,2,2,4),(0.60487773515436,
0.756090652495323,0.907303569836285,1.0585295200725,1.20975547030872),
 .UNSPECIFIED.);
#437=B_SPLINE_CURVE_WITH_KNOTS('',3,(#1622,#1623,#1624,#1625,#1626,#1627,
#1628,#1629,#1630,#1631),.UNSPECIFIED.,.F.,.F.,(4,2,2,2,4),(-1.20891094744703,
-1.05779284509095,-0.906674742734871,-0.755565108229192,-0.604455473723513),
 .UNSPECIFIED.);
#438=B_SPLINE_CURVE_WITH_KNOTS('',3,(#1635,#1636,#1637,#1638,#1639,#1640,
#1641,#1642,#1643,#1644,#1645,#1646,#1647,#1648,#1649,#1650,#1651,#1652),
 .UNSPECIFIED.,.F.,.F.,(4,2,2,2,2,2,2,2,4),(-2.41951094061744,-2.26828499038122,
-2.11705904014501,-1.96584612280404,-1.81463320546308,-1.66342028812212,
-1.51220737078115,-1.36098142054494,-1.20975547030872),.UNSPECIFIED.);
#439=B_SPLINE_CURVE_WITH_KNOTS('',3,(#1653,#1654,#1655,#1656,#1657,#1658,
#1659,#1660,#1661,#1662,#1663,#1664,#1665,#1666,#1667,#1668,#1669,#1670),
 .UNSPECIFIED.,.F.,.F.,(4,2,2,2,2,2,2,2,4),(-1.20975547030872,-1.0585295200725,
-0.907303569836286,-0.756090652495323,-0.60487773515436,-0.453664817813397,
-0.302451900472434,-0.151225950236217,0.),.UNSPECIFIED.);
#440=B_SPLINE_CURVE_WITH_KNOTS('',3,(#1674,#1675,#1676,#1677,#1678,#1679,
#1680,#1681,#1682,#1683,#1684,#1685,#1686,#1687,#1688,#1689,#1690,#1691),
 .UNSPECIFIED.,.F.,.F.,(4,2,2,2,2,2,2,2,4),(0.,0.151118102356077,0.302236204712155,
0.453345839217834,0.604455473723513,0.755565108229192,0.906674742734871,
1.05779284509095,1.20891094744703),.UNSPECIFIED.);
#441=B_SPLINE_CURVE_WITH_KNOTS('',3,(#1692,#1693,#1694,#1695,#1696,#1697,
#1698,#1699,#1700,#1701,#1702,#1703,#1704,#1705,#1706,#1707,#1708,#1709),
 .UNSPECIFIED.,.F.,.F.,(4,2,2,2,2,2,2,2,4),(1.20891094744703,1.3600290498031,
1.51114715215918,1.66225678666486,1.81336642117054,1.96447605567622,2.1155856901819,
2.26670379253797,2.41782189489405),.UNSPECIFIED.);
#442=B_SPLINE_CURVE_WITH_KNOTS('',3,(#1805,#1806,#1807,#1808,#1809,#1810,
#1811,#1812,#1813,#1814,#1815,#1816,#1817,#1818,#1819,#1820,#1821,#1822,
#1823),.UNSPECIFIED.,.F.,.F.,(4,3,3,3,3,3,4),(0.,0.25,0.625,0.869068416619454,
0.996324238316631,1.,1.03680973061555),.UNSPECIFIED.);
#443=B_SPLINE_CURVE_WITH_KNOTS('',3,(#1824,#1825,#1826,#1827,#1828,#1829,
#1830,#1831,#1832,#1833,#1834,#1835,#1836,#1837,#1838,#1839,#1840,#1841,
#1842),.UNSPECIFIED.,.F.,.F.,(4,3,3,3,3,3,4),(-1.03680973061555,-1.,-0.996324238316631,
-0.869068416619454,-0.625,-0.25,0.),.UNSPECIFIED.);
#444=B_SPLINE_CURVE_WITH_KNOTS('',5,(#1894,#1895,#1896,#1897,#1898,#1899,
#1900,#1901,#1902,#1903,#1904,#1905,#1906,#1907,#1908,#1909,#1910,#1911,
#1912,#1913,#1914,#1915,#1916,#1917),.UNSPECIFIED.,.F.,.F.,(6,1,1,1,1,1,
1,1,1,1,1,1,1,1,1,4,6),(0.,0.0666666666666667,0.133333333333333,0.2,0.266666666666667,
0.333333333333333,0.4,0.466666666666667,0.533333333333333,0.6,0.666666666666667,
0.733333333333333,0.8,0.866666666666667,0.933333333333333,1.,1.04017974969531),
 .UNSPECIFIED.);
#445=B_SPLINE_CURVE_WITH_KNOTS('',5,(#1920,#1921,#1922,#1923,#1924,#1925,
#1926,#1927,#1928,#1929,#1930,#1931,#1932,#1933,#1934,#1935,#1936,#1937,
#1938,#1939,#1940,#1941,#1942,#1943),.UNSPECIFIED.,.F.,.F.,(6,1,1,1,1,1,
1,1,1,1,1,1,1,1,1,4,6),(0.,0.0666666666666667,0.133333333333333,0.2,0.266666666666667,
0.333333333333333,0.4,0.466666666666667,0.533333333333333,0.6,0.666666666666667,
0.733333333333333,0.8,0.866666666666667,0.933333333333333,1.,1.04017974969531),
 .UNSPECIFIED.);
#446=B_SPLINE_CURVE_WITH_KNOTS('',3,(#1946,#1947,#1948,#1949,#1950,#1951,
#1952,#1953,#1954,#1955,#1956,#1957,#1958,#1959,#1960,#1961,#1962,#1963,
#1964),.UNSPECIFIED.,.F.,.F.,(4,3,3,3,3,3,4),(-1.03680973061555,-1.,-0.996324238316733,
-0.869068416619454,-0.625,-0.25,0.),.UNSPECIFIED.);
#447=B_SPLINE_CURVE_WITH_KNOTS('',5,(#1971,#1972,#1973,#1974,#1975,#1976,
#1977,#1978,#1979,#1980,#1981,#1982,#1983,#1984,#1985,#1986,#1987,#1988,
#1989,#1990,#1991,#1992,#1993,#1994),.UNSPECIFIED.,.F.,.F.,(6,4,1,1,1,1,
1,1,1,1,1,1,1,1,1,1,6),(-1.04017974969531,-1.,-0.933333333333333,-0.866666666666667,
-0.8,-0.733333333333333,-0.666666666666667,-0.6,-0.533333333333333,-0.466666666666667,
-0.4,-0.333333333333333,-0.266666666666667,-0.2,-0.133333333333333,-0.0666666666666667,
0.),.UNSPECIFIED.);
#448=B_SPLINE_CURVE_WITH_KNOTS('',5,(#1997,#1998,#1999,#2000,#2001,#2002,
#2003,#2004,#2005,#2006,#2007,#2008,#2009,#2010,#2011,#2012,#2013,#2014,
#2015,#2016,#2017,#2018,#2019,#2020),.UNSPECIFIED.,.F.,.F.,(6,4,1,1,1,1,
1,1,1,1,1,1,1,1,1,1,6),(-1.04017974969531,-1.,-0.933333333333333,-0.866666666666667,
-0.8,-0.733333333333333,-0.666666666666667,-0.6,-0.533333333333333,-0.466666666666667,
-0.4,-0.333333333333333,-0.266666666666667,-0.2,-0.133333333333333,-0.0666666666666667,
0.),.UNSPECIFIED.);
#449=B_SPLINE_CURVE_WITH_KNOTS('',3,(#2027,#2028,#2029,#2030,#2031,#2032,
#2033,#2034,#2035,#2036,#2037,#2038,#2039,#2040,#2041,#2042,#2043,#2044,
#2045),.UNSPECIFIED.,.F.,.F.,(4,3,3,3,3,3,4),(0.,0.25,0.625,0.869068416619454,
0.996324238316733,1.,1.03680973061555),.UNSPECIFIED.);
#450=B_SPLINE_CURVE_WITH_KNOTS('',5,(#2270,#2271,#2272,#2273,#2274,#2275,
#2276,#2277,#2278,#2279,#2280,#2281,#2282,#2283,#2284,#2285,#2286,#2287,
#2288,#2289),.UNSPECIFIED.,.F.,.F.,(6,1,1,1,1,1,1,1,1,1,1,1,1,1,1,6),(0.,
0.0666666666666667,0.133333333333333,0.2,0.266666666666667,0.333333333333333,
0.4,0.466666666666667,0.533333333333333,0.6,0.666666666666667,0.733333333333333,
0.8,0.866666666666667,0.933333333333333,1.),.UNSPECIFIED.);
#451=B_SPLINE_CURVE_WITH_KNOTS('',5,(#2291,#2292,#2293,#2294,#2295,#2296,
#2297,#2298,#2299,#2300,#2301,#2302,#2303,#2304,#2305,#2306,#2307,#2308,
#2309,#2310),.UNSPECIFIED.,.F.,.F.,(6,1,1,1,1,1,1,1,1,1,1,1,1,1,1,6),(-1.,
-0.933333333333333,-0.866666666666667,-0.8,-0.733333333333333,-0.666666666666667,
-0.6,-0.533333333333333,-0.466666666666667,-0.4,-0.333333333333333,-0.266666666666667,
-0.2,-0.133333333333333,-0.0666666666666667,0.),.UNSPECIFIED.);
#452=B_SPLINE_CURVE_WITH_KNOTS('',3,(#2318,#2319,#2320,#2321,#2322,#2323,
#2324,#2325,#2326,#2327),.UNSPECIFIED.,.F.,.F.,(4,2,2,2,4),(0.,0.249999999999997,
0.624999999999999,0.869068416619453,0.996324238316733),.UNSPECIFIED.);
#453=B_SPLINE_CURVE_WITH_KNOTS('',3,(#2329,#2330,#2331,#2332,#2333,#2334,
#2335,#2336,#2337,#2338),.UNSPECIFIED.,.F.,.F.,(4,2,2,2,4),(-0.996324238316631,
-0.869068416619454,-0.625,-0.25,0.),.UNSPECIFIED.);
#454=B_SPLINE_CURVE_WITH_KNOTS('',5,(#2385,#2386,#2387,#2388,#2389,#2390,
#2391,#2392,#2393,#2394,#2395,#2396,#2397,#2398,#2399,#2400,#2401,#2402,
#2403,#2404),.UNSPECIFIED.,.F.,.F.,(6,1,1,1,1,1,1,1,1,1,1,1,1,1,1,6),(-1.,
-0.933333333333333,-0.866666666666667,-0.8,-0.733333333333333,-0.666666666666667,
-0.6,-0.533333333333333,-0.466666666666667,-0.4,-0.333333333333333,-0.266666666666667,
-0.2,-0.133333333333333,-0.0666666666666667,0.),.UNSPECIFIED.);
#455=B_SPLINE_CURVE_WITH_KNOTS('',5,(#2447,#2448,#2449,#2450,#2451,#2452,
#2453,#2454,#2455,#2456,#2457,#2458,#2459,#2460,#2461,#2462,#2463,#2464,
#2465,#2466),.UNSPECIFIED.,.F.,.F.,(6,1,1,1,1,1,1,1,1,1,1,1,1,1,1,6),(0.,
0.0666666666666667,0.133333333333333,0.2,0.266666666666667,0.333333333333333,
0.4,0.466666666666667,0.533333333333333,0.6,0.666666666666667,0.733333333333333,
0.8,0.866666666666667,0.933333333333333,1.),.UNSPECIFIED.);
#456=B_SPLINE_CURVE_WITH_KNOTS('',3,(#2507,#2508,#2509,#2510,#2511,#2512,
#2513,#2514,#2515,#2516),.UNSPECIFIED.,.F.,.F.,(4,2,2,2,4),(-0.996324238316733,
-0.869068416619454,-0.625,-0.25,0.),.UNSPECIFIED.);
#457=B_SPLINE_CURVE_WITH_KNOTS('',3,(#2545,#2546,#2547,#2548,#2549,#2550,
#2551,#2552,#2553,#2554),.UNSPECIFIED.,.F.,.F.,(4,2,2,2,4),(0.,0.25,0.625,
0.869068416619454,0.996324238316631),.UNSPECIFIED.);
#458=B_SPLINE_CURVE_WITH_KNOTS('',3,(#2612,#2613,#2614,#2615,#2616,#2617,
#2618,#2619,#2620,#2621,#2622,#2623,#2624,#2625,#2626,#2627,#2628,#2629),
 .UNSPECIFIED.,.F.,.F.,(4,2,2,2,2,2,2,2,4),(0.,0.15103927001047,0.30207854002094,
0.45311206771438,0.604145595407819,0.755179123101259,0.906212650794699,
1.05725192080517,1.20829119081564),.UNSPECIFIED.);
#459=B_SPLINE_CURVE_WITH_KNOTS('',3,(#2630,#2631,#2632,#2633,#2634,#2635,
#2636,#2637,#2638,#2639,#2640,#2641,#2642,#2643,#2644,#2645,#2646,#2647),
 .UNSPECIFIED.,.F.,.F.,(4,2,2,2,2,2,2,2,4),(1.20829119081564,1.35933046082611,
1.51036973083658,1.66140325853002,1.81243678622346,1.9634703139169,2.11450384161034,
2.26554311162081,2.41658238163128),.UNSPECIFIED.);
#460=B_SPLINE_CURVE_WITH_KNOTS('',3,(#2651,#2652,#2653,#2654,#2655,#2656,
#2657,#2658,#2659,#2660,#2661,#2662,#2663,#2664,#2665,#2666,#2667,#2668),
 .UNSPECIFIED.,.F.,.F.,(4,2,2,2,2,2,2,2,4),(0.,0.151118102356077,0.302236204712155,
0.453345839217834,0.604455473723513,0.755565108229192,0.906674742734871,
1.05779284509095,1.20891094744703),.UNSPECIFIED.);
#461=B_SPLINE_CURVE_WITH_KNOTS('',3,(#2669,#2670,#2671,#2672,#2673,#2674,
#2675,#2676,#2677,#2678,#2679,#2680,#2681,#2682,#2683,#2684,#2685,#2686),
 .UNSPECIFIED.,.F.,.F.,(4,2,2,2,2,2,2,2,4),(1.20891094744703,1.3600290498031,
1.51114715215918,1.66225678666486,1.81336642117054,1.96447605567622,2.1155856901819,
2.26670379253797,2.41782189489405),.UNSPECIFIED.);
#462=B_SPLINE_CURVE_WITH_KNOTS('',3,(#2690,#2691,#2692,#2693,#2694,#2695,
#2696,#2697,#2698,#2699),.UNSPECIFIED.,.F.,.F.,(4,2,2,2,4),(0.,0.151118102356077,
0.302236204712155,0.453345839217834,0.604455473723513),.UNSPECIFIED.);
#463=B_SPLINE_CURVE_WITH_KNOTS('',3,(#2701,#2702,#2703,#2704,#2705,#2706,
#2707,#2708,#2709,#2710),.UNSPECIFIED.,.F.,.F.,(4,2,2,2,4),(1.81336642117054,
1.96447605567622,2.1155856901819,2.26670379253797,2.41782189489405),
 .UNSPECIFIED.);
#464=B_SPLINE_CURVE_WITH_KNOTS('',3,(#2712,#2713,#2714,#2715,#2716,#2717,
#2718,#2719,#2720,#2721),.UNSPECIFIED.,.F.,.F.,(4,2,2,2,4),(1.20891094744703,
1.3600290498031,1.51114715215918,1.66225678666486,1.81336642117054),
 .UNSPECIFIED.);
#465=B_SPLINE_CURVE_WITH_KNOTS('',3,(#2725,#2726,#2727,#2728,#2729,#2730,
#2731,#2732,#2733,#2734),.UNSPECIFIED.,.F.,.F.,(4,2,2,2,4),(0.604145595407819,
0.755179123101259,0.906212650794699,1.05725192080517,1.20829119081564),
 .UNSPECIFIED.);
#466=B_SPLINE_CURVE_WITH_KNOTS('',3,(#2736,#2737,#2738,#2739,#2740,#2741,
#2742,#2743,#2744,#2745),.UNSPECIFIED.,.F.,.F.,(4,2,2,2,4),(0.,0.15103927001047,
0.30207854002094,0.45311206771438,0.604145595407819),.UNSPECIFIED.);
#467=B_SPLINE_CURVE_WITH_KNOTS('',3,(#2747,#2748,#2749,#2750,#2751,#2752,
#2753,#2754,#2755,#2756),.UNSPECIFIED.,.F.,.F.,(4,2,2,2,4),(1.81243678622346,
1.9634703139169,2.11450384161034,2.26554311162081,2.41658238163128),
 .UNSPECIFIED.);
#468=B_SPLINE_CURVE_WITH_KNOTS('',3,(#2757,#2758,#2759,#2760,#2761,#2762,
#2763,#2764,#2765,#2766),.UNSPECIFIED.,.F.,.F.,(4,2,2,2,4),(1.20829119081564,
1.35933046082611,1.51036973083658,1.66140325853002,1.81243678622346),
 .UNSPECIFIED.);
#469=B_SPLINE_CURVE_WITH_KNOTS('',3,(#2767,#2768,#2769,#2770,#2771,#2772,
#2773,#2774,#2775,#2776),.UNSPECIFIED.,.F.,.F.,(4,2,2,2,4),(0.604455473723513,
0.755565108229192,0.906674742734871,1.05779284509095,1.20891094744703),
 .UNSPECIFIED.);
#470=B_SPLINE_CURVE_WITH_KNOTS('',3,(#2852,#2853,#2854,#2855,#2856,#2857,
#2858,#2859,#2860,#2861,#2862,#2863,#2864,#2865,#2866,#2867,#2868,#2869,
#2870,#2871,#2872,#2873,#2874,#2875,#2876,#2877,#2878,#2879,#2880,#2881,
#2882,#2883,#2884,#2885,#2886,#2887,#2888,#2889,#2890),.UNSPECIFIED.,.T.,
 .F.,(4,2,2,2,2,2,2,2,2,3,2,2,2,2,2,2,2,2,4),(-1.22336998493156,-1.09724704826145,
-0.94233260352668,-0.819540701938356,-0.665268805075334,-0.532997978376738,
-0.416879806790855,-0.348119554508441,-0.194082006902748,0.,0.0915534191865666,
0.143556411629729,0.19120578161277,0.250961021394097,0.349888531367616,
0.483105049112713,0.64448257383362,0.847091969730186,0.943107169338909),
 .UNSPECIFIED.);
#471=B_SPLINE_CURVE_WITH_KNOTS('',3,(#2893,#2894,#2895,#2896,#2897,#2898,
#2899,#2900,#2901,#2902,#2903,#2904,#2905,#2906,#2907,#2908,#2909,#2910,
#2911,#2912,#2913,#2914,#2915,#2916,#2917,#2918,#2919,#2920,#2921,#2922,
#2923,#2924,#2925,#2926,#2927,#2928,#2929,#2930,#2931),.UNSPECIFIED.,.T.,
 .F.,(4,2,2,2,2,2,2,2,2,3,2,2,2,2,2,2,2,2,4),(0.841924175679887,0.899224077974559,
1.04154799590402,1.16552064731243,1.2634318988501,1.33413129228483,1.38504379679693,
1.43998123008145,1.50705480177247,1.5985340249232,1.78874148499628,1.89884515666463,
1.94059180293314,2.00808103022965,2.08168057719367,2.18184892200529,2.26512781300167,
2.36548642654063,2.44045820060308),.UNSPECIFIED.);
#472=B_SPLINE_CURVE_WITH_KNOTS('',3,(#3008,#3009,#3010,#3011,#3012,#3013,
#3014,#3015,#3016,#3017,#3018,#3019,#3020,#3021),.UNSPECIFIED.,.F.,.F.,
(4,2,2,2,2,2,4),(-8.38846342825229,-7.81059488838674,-7.33125287845917,
-6.97540830612223,-6.24864745818615,-5.47486898738129,-5.43941055956934),
 .UNSPECIFIED.);
#473=B_SPLINE_CURVE_WITH_KNOTS('',3,(#3025,#3026,#3027,#3028,#3029,#3030,
#3031,#3032,#3033,#3034,#3035,#3036),.UNSPECIFIED.,.F.,.F.,(4,2,2,2,2,4),
(-1.54762978928542,-1.4583177708316,-1.30106672545541,-1.0655082126291,
-0.772398014621137,-0.63986385113685),.UNSPECIFIED.);
#474=B_SPLINE_CURVE_WITH_KNOTS('',3,(#3038,#3039,#3040,#3041,#3042,#3043,
#3044,#3045,#3046,#3047,#3048,#3049,#3050,#3051,#3052,#3053,#3054,#3055,
#3056,#3057,#3058,#3059,#3060),.UNSPECIFIED.,.F.,.F.,(4,2,2,3,2,2,2,2,2,
2,4),(-0.63986385113685,-0.480616814211645,-0.224081253454166,0.,0.120874650966817,
0.237558789133194,0.404814120558448,0.574370503307451,0.750868718798978,
0.951765363187613,1.01851822860381),.UNSPECIFIED.);
#475=B_SPLINE_CURVE_WITH_KNOTS('',3,(#3061,#3062,#3063,#3064,#3065,#3066,
#3067,#3068,#3069,#3070,#3071,#3072),.UNSPECIFIED.,.F.,.F.,(4,2,2,2,2,4),
(1.01851822860381,1.24595614735538,1.70407595255937,2.11785747517733,2.45585059804079,
2.5337692675404),.UNSPECIFIED.);
#476=B_SPLINE_CURVE_WITH_KNOTS('',3,(#3074,#3075,#3076,#3077,#3078,#3079,
#3080,#3081,#3082,#3083,#3084,#3085),.UNSPECIFIED.,.F.,.F.,(4,2,2,2,2,4),
(-1.51818210876971,-1.27085914681692,-1.04616678368018,-0.601418643689676,
-0.233877903034561,-1.0000006369637E-6),.UNSPECIFIED.);
#477=B_SPLINE_CURVE_WITH_KNOTS('',3,(#3086,#3087,#3088,#3089,#3090,#3091,
#3092,#3093,#3094,#3095,#3096,#3097,#3098,#3099,#3100,#3101,#3102,#3103,
#3104,#3105),.UNSPECIFIED.,.F.,.F.,(4,2,2,2,2,2,2,2,2,4),(-5.43941055956934,
-4.53226345790708,-3.19238180995312,-2.23633703092198,-1.64902196252929,
-1.16164668394398,-0.707426447143085,-0.268000268469295,-0.112074736598375,
-9.99999999985594E-7),.UNSPECIFIED.);
#478=VERTEX_POINT('',#1547);
#479=VERTEX_POINT('',#1548);
#480=VERTEX_POINT('',#1568);
#481=VERTEX_POINT('',#1579);
#482=VERTEX_POINT('',#1581);
#483=VERTEX_POINT('',#1592);
#484=VERTEX_POINT('',#1633);
#485=VERTEX_POINT('',#1634);
#486=VERTEX_POINT('',#1671);
#487=VERTEX_POINT('',#1673);
#488=VERTEX_POINT('',#1711);
#489=VERTEX_POINT('',#1714);
#490=VERTEX_POINT('',#1718);
#491=VERTEX_POINT('',#1721);
#492=VERTEX_POINT('',#1728);
#493=VERTEX_POINT('',#1731);
#494=VERTEX_POINT('',#1735);
#495=VERTEX_POINT('',#1737);
#496=VERTEX_POINT('',#1744);
#497=VERTEX_POINT('',#1745);
#498=VERTEX_POINT('',#1747);
#499=VERTEX_POINT('',#1749);
#500=VERTEX_POINT('',#1753);
#501=VERTEX_POINT('',#1754);
#502=VERTEX_POINT('',#1759);
#503=VERTEX_POINT('',#1760);
#504=VERTEX_POINT('',#1802);
#505=VERTEX_POINT('',#1803);
#506=VERTEX_POINT('',#1893);
#507=VERTEX_POINT('',#1918);
#508=VERTEX_POINT('',#1945);
#509=VERTEX_POINT('',#1965);
#510=VERTEX_POINT('',#1967);
#511=VERTEX_POINT('',#1969);
#512=VERTEX_POINT('',#1996);
#513=VERTEX_POINT('',#2021);
#514=VERTEX_POINT('',#2023);
#515=VERTEX_POINT('',#2025);
#516=VERTEX_POINT('',#2169);
#517=VERTEX_POINT('',#2170);
#518=VERTEX_POINT('',#2173);
#519=VERTEX_POINT('',#2177);
#520=VERTEX_POINT('',#2210);
#521=VERTEX_POINT('',#2211);
#522=VERTEX_POINT('',#2214);
#523=VERTEX_POINT('',#2218);
#524=VERTEX_POINT('',#2251);
#525=VERTEX_POINT('',#2252);
#526=VERTEX_POINT('',#2254);
#527=VERTEX_POINT('',#2259);
#528=VERTEX_POINT('',#2266);
#529=VERTEX_POINT('',#2267);
#530=VERTEX_POINT('',#2269);
#531=VERTEX_POINT('',#2290);
#532=VERTEX_POINT('',#2311);
#533=VERTEX_POINT('',#2313);
#534=VERTEX_POINT('',#2315);
#535=VERTEX_POINT('',#2317);
#536=VERTEX_POINT('',#2328);
#537=VERTEX_POINT('',#2339);
#538=VERTEX_POINT('',#2382);
#539=VERTEX_POINT('',#2384);
#540=VERTEX_POINT('',#2446);
#541=VERTEX_POINT('',#2469);
#542=VERTEX_POINT('',#2473);
#543=VERTEX_POINT('',#2477);
#544=VERTEX_POINT('',#2506);
#545=VERTEX_POINT('',#2544);
#546=VERTEX_POINT('',#2557);
#547=VERTEX_POINT('',#2561);
#548=VERTEX_POINT('',#2595);
#549=VERTEX_POINT('',#2596);
#550=VERTEX_POINT('',#2598);
#551=VERTEX_POINT('',#2603);
#552=VERTEX_POINT('',#2610);
#553=VERTEX_POINT('',#2611);
#554=VERTEX_POINT('',#2648);
#555=VERTEX_POINT('',#2650);
#556=VERTEX_POINT('',#2688);
#557=VERTEX_POINT('',#2689);
#558=VERTEX_POINT('',#2700);
#559=VERTEX_POINT('',#2711);
#560=VERTEX_POINT('',#2722);
#561=VERTEX_POINT('',#2724);
#562=VERTEX_POINT('',#2735);
#563=VERTEX_POINT('',#2746);
#564=VERTEX_POINT('',#2851);
#565=VERTEX_POINT('',#2891);
#566=VERTEX_POINT('',#3006);
#567=VERTEX_POINT('',#3007);
#568=VERTEX_POINT('',#3022);
#569=VERTEX_POINT('',#3024);
#570=VERTEX_POINT('',#3037);
#571=VERTEX_POINT('',#3073);
#572=VERTEX_POINT('',#3107);
#573=VERTEX_POINT('',#3109);
#574=VERTEX_POINT('',#3114);
#575=VERTEX_POINT('',#3118);
#576=EDGE_CURVE('',#478,#479,#432,.F.);
#577=EDGE_CURVE('',#480,#478,#433,.F.);
#578=EDGE_CURVE('',#480,#481,#300,.T.);
#579=EDGE_CURVE('',#482,#481,#434,.F.);
#580=EDGE_CURVE('',#483,#482,#435,.F.);
#581=EDGE_CURVE('',#481,#483,#436,.F.);
#582=EDGE_CURVE('',#479,#480,#437,.F.);
#583=EDGE_CURVE('',#484,#485,#438,.T.);
#584=EDGE_CURVE('',#485,#484,#439,.T.);
#585=EDGE_CURVE('',#485,#486,#301,.T.);
#586=EDGE_CURVE('',#487,#486,#440,.T.);
#587=EDGE_CURVE('',#486,#487,#441,.T.);
#588=EDGE_CURVE('',#488,#488,#139,.T.);
#589=EDGE_CURVE('',#488,#482,#302,.T.);
#590=EDGE_CURVE('',#483,#489,#303,.T.);
#591=EDGE_CURVE('',#489,#489,#140,.T.);
#592=EDGE_CURVE('',#490,#490,#141,.T.);
#593=EDGE_CURVE('',#490,#479,#304,.T.);
#594=EDGE_CURVE('',#478,#491,#305,.T.);
#595=EDGE_CURVE('',#491,#491,#142,.T.);
#596=EDGE_CURVE('',#492,#492,#143,.T.);
#597=EDGE_CURVE('',#492,#493,#306,.T.);
#598=EDGE_CURVE('',#493,#493,#144,.T.);
#599=EDGE_CURVE('',#494,#494,#145,.T.);
#600=EDGE_CURVE('',#494,#495,#307,.T.);
#601=EDGE_CURVE('',#495,#495,#146,.T.);
#602=EDGE_CURVE('',#496,#497,#308,.T.);
#603=EDGE_CURVE('',#498,#497,#309,.T.);
#604=EDGE_CURVE('',#498,#499,#310,.T.);
#605=EDGE_CURVE('',#496,#499,#311,.T.);
#606=EDGE_CURVE('',#500,#501,#312,.T.);
#607=EDGE_CURVE('',#497,#501,#313,.T.);
#608=EDGE_CURVE('',#500,#496,#314,.T.);
#609=EDGE_CURVE('',#502,#503,#315,.T.);
#610=EDGE_CURVE('',#501,#503,#316,.T.);
#611=EDGE_CURVE('',#502,#500,#317,.T.);
#612=EDGE_CURVE('',#504,#505,#318,.F.);
#613=EDGE_CURVE('',#503,#505,#442,.T.);
#614=EDGE_CURVE('',#504,#502,#443,.T.);
#615=EDGE_CURVE('',#506,#498,#444,.F.);
#616=EDGE_CURVE('',#507,#506,#319,.F.);
#617=EDGE_CURVE('',#499,#507,#445,.T.);
#618=EDGE_CURVE('',#505,#508,#446,.T.);
#619=EDGE_CURVE('',#508,#509,#320,.T.);
#620=EDGE_CURVE('',#509,#510,#321,.T.);
#621=EDGE_CURVE('',#510,#511,#322,.T.);
#622=EDGE_CURVE('',#511,#506,#447,.F.);
#623=EDGE_CURVE('',#507,#512,#448,.T.);
#624=EDGE_CURVE('',#512,#513,#323,.T.);
#625=EDGE_CURVE('',#513,#514,#324,.T.);
#626=EDGE_CURVE('',#514,#515,#325,.T.);
#627=EDGE_CURVE('',#515,#504,#449,.T.);
#628=EDGE_CURVE('',#512,#511,#326,.T.);
#629=EDGE_CURVE('',#513,#510,#327,.T.);
#630=EDGE_CURVE('',#514,#509,#328,.T.);
#631=EDGE_CURVE('',#515,#508,#329,.T.);
#632=EDGE_CURVE('',#516,#517,#147,.T.);
#633=EDGE_CURVE('',#517,#516,#148,.T.);
#634=EDGE_CURVE('',#517,#518,#149,.T.);
#635=EDGE_CURVE('',#518,#518,#150,.T.);
#636=EDGE_CURVE('',#519,#519,#151,.T.);
#637=EDGE_CURVE('',#519,#516,#330,.T.);
#638=EDGE_CURVE('',#520,#521,#152,.T.);
#639=EDGE_CURVE('',#521,#520,#153,.T.);
#640=EDGE_CURVE('',#521,#522,#154,.T.);
#641=EDGE_CURVE('',#522,#522,#155,.T.);
#642=EDGE_CURVE('',#523,#523,#156,.T.);
#643=EDGE_CURVE('',#523,#520,#331,.T.);
#644=EDGE_CURVE('',#524,#525,#157,.T.);
#645=EDGE_CURVE('',#525,#526,#158,.T.);
#646=EDGE_CURVE('',#526,#526,#159,.T.);
#647=EDGE_CURVE('',#525,#524,#160,.T.);
#648=EDGE_CURVE('',#524,#527,#332,.T.);
#649=EDGE_CURVE('',#527,#527,#161,.T.);
#650=EDGE_CURVE('',#528,#529,#333,.T.);
#651=EDGE_CURVE('',#529,#530,#450,.T.);
#652=EDGE_CURVE('',#530,#531,#451,.T.);
#653=EDGE_CURVE('',#531,#532,#334,.T.);
#654=EDGE_CURVE('',#532,#533,#335,.T.);
#655=EDGE_CURVE('',#533,#534,#336,.T.);
#656=EDGE_CURVE('',#534,#535,#452,.T.);
#657=EDGE_CURVE('',#535,#536,#453,.T.);
#658=EDGE_CURVE('',#536,#537,#337,.T.);
#659=EDGE_CURVE('',#537,#528,#338,.T.);
#660=EDGE_CURVE('',#538,#529,#339,.T.);
#661=EDGE_CURVE('',#539,#538,#454,.T.);
#662=EDGE_CURVE('',#530,#539,#340,.T.);
#663=EDGE_CURVE('',#540,#539,#455,.T.);
#664=EDGE_CURVE('',#531,#540,#341,.T.);
#665=EDGE_CURVE('',#541,#540,#342,.T.);
#666=EDGE_CURVE('',#532,#541,#343,.T.);
#667=EDGE_CURVE('',#542,#541,#344,.T.);
#668=EDGE_CURVE('',#533,#542,#345,.T.);
#669=EDGE_CURVE('',#543,#542,#346,.T.);
#670=EDGE_CURVE('',#534,#543,#347,.T.);
#671=EDGE_CURVE('',#544,#543,#456,.T.);
#672=EDGE_CURVE('',#535,#544,#348,.T.);
#673=EDGE_CURVE('',#545,#544,#457,.T.);
#674=EDGE_CURVE('',#536,#545,#349,.T.);
#675=EDGE_CURVE('',#546,#545,#350,.T.);
#676=EDGE_CURVE('',#537,#546,#351,.T.);
#677=EDGE_CURVE('',#547,#546,#352,.T.);
#678=EDGE_CURVE('',#528,#547,#353,.T.);
#679=EDGE_CURVE('',#538,#547,#354,.T.);
#680=EDGE_CURVE('',#548,#549,#162,.T.);
#681=EDGE_CURVE('',#549,#550,#163,.T.);
#682=EDGE_CURVE('',#550,#550,#164,.T.);
#683=EDGE_CURVE('',#549,#548,#165,.T.);
#684=EDGE_CURVE('',#548,#551,#355,.T.);
#685=EDGE_CURVE('',#551,#551,#166,.T.);
#686=EDGE_CURVE('',#552,#553,#458,.T.);
#687=EDGE_CURVE('',#553,#552,#459,.T.);
#688=EDGE_CURVE('',#553,#554,#356,.T.);
#689=EDGE_CURVE('',#555,#554,#460,.T.);
#690=EDGE_CURVE('',#554,#555,#461,.T.);
#691=EDGE_CURVE('',#556,#557,#462,.T.);
#692=EDGE_CURVE('',#558,#556,#463,.T.);
#693=EDGE_CURVE('',#559,#558,#464,.T.);
#694=EDGE_CURVE('',#559,#560,#357,.T.);
#695=EDGE_CURVE('',#561,#560,#465,.T.);
#696=EDGE_CURVE('',#562,#561,#466,.T.);
#697=EDGE_CURVE('',#563,#562,#467,.T.);
#698=EDGE_CURVE('',#560,#563,#468,.T.);
#699=EDGE_CURVE('',#557,#559,#469,.T.);
#700=EDGE_CURVE('',#564,#564,#470,.T.);
#701=EDGE_CURVE('',#564,#565,#358,.T.);
#702=EDGE_CURVE('',#565,#565,#471,.T.);
#703=EDGE_CURVE('',#566,#567,#472,.T.);
#704=EDGE_CURVE('',#568,#566,#359,.T.);
#705=EDGE_CURVE('',#569,#568,#473,.F.);
#706=EDGE_CURVE('',#570,#569,#474,.F.);
#707=EDGE_CURVE('',#568,#570,#475,.F.);
#708=EDGE_CURVE('',#571,#566,#476,.T.);
#709=EDGE_CURVE('',#567,#571,#477,.T.);
#710=EDGE_CURVE('',#572,#572,#167,.T.);
#711=EDGE_CURVE('',#573,#573,#168,.T.);
#712=EDGE_CURVE('',#573,#571,#360,.T.);
#713=EDGE_CURVE('',#567,#558,#361,.T.);
#714=EDGE_CURVE('',#557,#574,#362,.T.);
#715=EDGE_CURVE('',#574,#574,#169,.T.);
#716=EDGE_CURVE('',#575,#575,#170,.T.);
#717=EDGE_CURVE('',#575,#563,#363,.T.);
#718=EDGE_CURVE('',#561,#569,#364,.T.);
#719=EDGE_CURVE('',#570,#572,#365,.T.);
#720=ORIENTED_EDGE('',*,*,#576,.F.);
#721=ORIENTED_EDGE('',*,*,#577,.F.);
#722=ORIENTED_EDGE('',*,*,#578,.T.);
#723=ORIENTED_EDGE('',*,*,#579,.F.);
#724=ORIENTED_EDGE('',*,*,#580,.F.);
#725=ORIENTED_EDGE('',*,*,#581,.F.);
#726=ORIENTED_EDGE('',*,*,#578,.F.);
#727=ORIENTED_EDGE('',*,*,#582,.F.);
#728=ORIENTED_EDGE('',*,*,#583,.F.);
#729=ORIENTED_EDGE('',*,*,#584,.F.);
#730=ORIENTED_EDGE('',*,*,#585,.T.);
#731=ORIENTED_EDGE('',*,*,#586,.F.);
#732=ORIENTED_EDGE('',*,*,#587,.F.);
#733=ORIENTED_EDGE('',*,*,#585,.F.);
#734=ORIENTED_EDGE('',*,*,#588,.T.);
#735=ORIENTED_EDGE('',*,*,#589,.T.);
#736=ORIENTED_EDGE('',*,*,#579,.T.);
#737=ORIENTED_EDGE('',*,*,#581,.T.);
#738=ORIENTED_EDGE('',*,*,#590,.T.);
#739=ORIENTED_EDGE('',*,*,#591,.F.);
#740=ORIENTED_EDGE('',*,*,#590,.F.);
#741=ORIENTED_EDGE('',*,*,#580,.T.);
#742=ORIENTED_EDGE('',*,*,#589,.F.);
#743=ORIENTED_EDGE('',*,*,#583,.T.);
#744=ORIENTED_EDGE('',*,*,#584,.T.);
#745=ORIENTED_EDGE('',*,*,#592,.F.);
#746=ORIENTED_EDGE('',*,*,#593,.T.);
#747=ORIENTED_EDGE('',*,*,#582,.T.);
#748=ORIENTED_EDGE('',*,*,#577,.T.);
#749=ORIENTED_EDGE('',*,*,#594,.T.);
#750=ORIENTED_EDGE('',*,*,#595,.T.);
#751=ORIENTED_EDGE('',*,*,#594,.F.);
#752=ORIENTED_EDGE('',*,*,#576,.T.);
#753=ORIENTED_EDGE('',*,*,#593,.F.);
#754=ORIENTED_EDGE('',*,*,#586,.T.);
#755=ORIENTED_EDGE('',*,*,#587,.T.);
#756=ORIENTED_EDGE('',*,*,#592,.T.);
#757=ORIENTED_EDGE('',*,*,#591,.T.);
#758=ORIENTED_EDGE('',*,*,#595,.F.);
#759=ORIENTED_EDGE('',*,*,#588,.F.);
#760=ORIENTED_EDGE('',*,*,#596,.F.);
#761=ORIENTED_EDGE('',*,*,#596,.T.);
#762=ORIENTED_EDGE('',*,*,#597,.T.);
#763=ORIENTED_EDGE('',*,*,#598,.F.);
#764=ORIENTED_EDGE('',*,*,#597,.F.);
#765=ORIENTED_EDGE('',*,*,#599,.F.);
#766=ORIENTED_EDGE('',*,*,#600,.T.);
#767=ORIENTED_EDGE('',*,*,#601,.F.);
#768=ORIENTED_EDGE('',*,*,#600,.F.);
#769=ORIENTED_EDGE('',*,*,#601,.T.);
#770=ORIENTED_EDGE('',*,*,#599,.T.);
#771=ORIENTED_EDGE('',*,*,#598,.T.);
#772=ORIENTED_EDGE('',*,*,#602,.T.);
#773=ORIENTED_EDGE('',*,*,#603,.F.);
#774=ORIENTED_EDGE('',*,*,#604,.T.);
#775=ORIENTED_EDGE('',*,*,#605,.F.);
#776=ORIENTED_EDGE('',*,*,#606,.T.);
#777=ORIENTED_EDGE('',*,*,#607,.F.);
#778=ORIENTED_EDGE('',*,*,#602,.F.);
#779=ORIENTED_EDGE('',*,*,#608,.F.);
#780=ORIENTED_EDGE('',*,*,#609,.T.);
#781=ORIENTED_EDGE('',*,*,#610,.F.);
#782=ORIENTED_EDGE('',*,*,#606,.F.);
#783=ORIENTED_EDGE('',*,*,#611,.F.);
#784=ORIENTED_EDGE('',*,*,#612,.T.);
#785=ORIENTED_EDGE('',*,*,#613,.F.);
#786=ORIENTED_EDGE('',*,*,#609,.F.);
#787=ORIENTED_EDGE('',*,*,#614,.F.);
#788=ORIENTED_EDGE('',*,*,#604,.F.);
#789=ORIENTED_EDGE('',*,*,#615,.F.);
#790=ORIENTED_EDGE('',*,*,#616,.F.);
#791=ORIENTED_EDGE('',*,*,#617,.F.);
#792=ORIENTED_EDGE('',*,*,#618,.T.);
#793=ORIENTED_EDGE('',*,*,#619,.T.);
#794=ORIENTED_EDGE('',*,*,#620,.T.);
#795=ORIENTED_EDGE('',*,*,#621,.T.);
#796=ORIENTED_EDGE('',*,*,#622,.T.);
#797=ORIENTED_EDGE('',*,*,#615,.T.);
#798=ORIENTED_EDGE('',*,*,#603,.T.);
#799=ORIENTED_EDGE('',*,*,#607,.T.);
#800=ORIENTED_EDGE('',*,*,#610,.T.);
#801=ORIENTED_EDGE('',*,*,#613,.T.);
#802=ORIENTED_EDGE('',*,*,#623,.T.);
#803=ORIENTED_EDGE('',*,*,#624,.T.);
#804=ORIENTED_EDGE('',*,*,#625,.T.);
#805=ORIENTED_EDGE('',*,*,#626,.T.);
#806=ORIENTED_EDGE('',*,*,#627,.T.);
#807=ORIENTED_EDGE('',*,*,#614,.T.);
#808=ORIENTED_EDGE('',*,*,#611,.T.);
#809=ORIENTED_EDGE('',*,*,#608,.T.);
#810=ORIENTED_EDGE('',*,*,#605,.T.);
#811=ORIENTED_EDGE('',*,*,#617,.T.);
#812=ORIENTED_EDGE('',*,*,#616,.T.);
#813=ORIENTED_EDGE('',*,*,#622,.F.);
#814=ORIENTED_EDGE('',*,*,#628,.F.);
#815=ORIENTED_EDGE('',*,*,#623,.F.);
#816=ORIENTED_EDGE('',*,*,#628,.T.);
#817=ORIENTED_EDGE('',*,*,#621,.F.);
#818=ORIENTED_EDGE('',*,*,#629,.F.);
#819=ORIENTED_EDGE('',*,*,#624,.F.);
#820=ORIENTED_EDGE('',*,*,#629,.T.);
#821=ORIENTED_EDGE('',*,*,#620,.F.);
#822=ORIENTED_EDGE('',*,*,#630,.F.);
#823=ORIENTED_EDGE('',*,*,#625,.F.);
#824=ORIENTED_EDGE('',*,*,#630,.T.);
#825=ORIENTED_EDGE('',*,*,#619,.F.);
#826=ORIENTED_EDGE('',*,*,#631,.F.);
#827=ORIENTED_EDGE('',*,*,#626,.F.);
#828=ORIENTED_EDGE('',*,*,#631,.T.);
#829=ORIENTED_EDGE('',*,*,#618,.F.);
#830=ORIENTED_EDGE('',*,*,#612,.F.);
#831=ORIENTED_EDGE('',*,*,#627,.F.);
#832=ORIENTED_EDGE('',*,*,#632,.F.);
#833=ORIENTED_EDGE('',*,*,#633,.F.);
#834=ORIENTED_EDGE('',*,*,#634,.T.);
#835=ORIENTED_EDGE('',*,*,#635,.F.);
#836=ORIENTED_EDGE('',*,*,#634,.F.);
#837=ORIENTED_EDGE('',*,*,#636,.F.);
#838=ORIENTED_EDGE('',*,*,#637,.T.);
#839=ORIENTED_EDGE('',*,*,#632,.T.);
#840=ORIENTED_EDGE('',*,*,#633,.T.);
#841=ORIENTED_EDGE('',*,*,#637,.F.);
#842=ORIENTED_EDGE('',*,*,#635,.T.);
#843=ORIENTED_EDGE('',*,*,#636,.T.);
#844=ORIENTED_EDGE('',*,*,#638,.F.);
#845=ORIENTED_EDGE('',*,*,#639,.F.);
#846=ORIENTED_EDGE('',*,*,#640,.T.);
#847=ORIENTED_EDGE('',*,*,#641,.F.);
#848=ORIENTED_EDGE('',*,*,#640,.F.);
#849=ORIENTED_EDGE('',*,*,#642,.F.);
#850=ORIENTED_EDGE('',*,*,#643,.T.);
#851=ORIENTED_EDGE('',*,*,#638,.T.);
#852=ORIENTED_EDGE('',*,*,#639,.T.);
#853=ORIENTED_EDGE('',*,*,#643,.F.);
#854=ORIENTED_EDGE('',*,*,#641,.T.);
#855=ORIENTED_EDGE('',*,*,#642,.T.);
#856=ORIENTED_EDGE('',*,*,#644,.T.);
#857=ORIENTED_EDGE('',*,*,#645,.T.);
#858=ORIENTED_EDGE('',*,*,#646,.T.);
#859=ORIENTED_EDGE('',*,*,#645,.F.);
#860=ORIENTED_EDGE('',*,*,#647,.T.);
#861=ORIENTED_EDGE('',*,*,#644,.F.);
#862=ORIENTED_EDGE('',*,*,#648,.T.);
#863=ORIENTED_EDGE('',*,*,#649,.T.);
#864=ORIENTED_EDGE('',*,*,#648,.F.);
#865=ORIENTED_EDGE('',*,*,#647,.F.);
#866=ORIENTED_EDGE('',*,*,#646,.F.);
#867=ORIENTED_EDGE('',*,*,#649,.F.);
#868=ORIENTED_EDGE('',*,*,#650,.T.);
#869=ORIENTED_EDGE('',*,*,#651,.T.);
#870=ORIENTED_EDGE('',*,*,#652,.T.);
#871=ORIENTED_EDGE('',*,*,#653,.T.);
#872=ORIENTED_EDGE('',*,*,#654,.T.);
#873=ORIENTED_EDGE('',*,*,#655,.T.);
#874=ORIENTED_EDGE('',*,*,#656,.T.);
#875=ORIENTED_EDGE('',*,*,#657,.T.);
#876=ORIENTED_EDGE('',*,*,#658,.T.);
#877=ORIENTED_EDGE('',*,*,#659,.T.);
#878=ORIENTED_EDGE('',*,*,#660,.F.);
#879=ORIENTED_EDGE('',*,*,#661,.F.);
#880=ORIENTED_EDGE('',*,*,#662,.F.);
#881=ORIENTED_EDGE('',*,*,#651,.F.);
#882=ORIENTED_EDGE('',*,*,#662,.T.);
#883=ORIENTED_EDGE('',*,*,#663,.F.);
#884=ORIENTED_EDGE('',*,*,#664,.F.);
#885=ORIENTED_EDGE('',*,*,#652,.F.);
#886=ORIENTED_EDGE('',*,*,#664,.T.);
#887=ORIENTED_EDGE('',*,*,#665,.F.);
#888=ORIENTED_EDGE('',*,*,#666,.F.);
#889=ORIENTED_EDGE('',*,*,#653,.F.);
#890=ORIENTED_EDGE('',*,*,#666,.T.);
#891=ORIENTED_EDGE('',*,*,#667,.F.);
#892=ORIENTED_EDGE('',*,*,#668,.F.);
#893=ORIENTED_EDGE('',*,*,#654,.F.);
#894=ORIENTED_EDGE('',*,*,#668,.T.);
#895=ORIENTED_EDGE('',*,*,#669,.F.);
#896=ORIENTED_EDGE('',*,*,#670,.F.);
#897=ORIENTED_EDGE('',*,*,#655,.F.);
#898=ORIENTED_EDGE('',*,*,#670,.T.);
#899=ORIENTED_EDGE('',*,*,#671,.F.);
#900=ORIENTED_EDGE('',*,*,#672,.F.);
#901=ORIENTED_EDGE('',*,*,#656,.F.);
#902=ORIENTED_EDGE('',*,*,#672,.T.);
#903=ORIENTED_EDGE('',*,*,#673,.F.);
#904=ORIENTED_EDGE('',*,*,#674,.F.);
#905=ORIENTED_EDGE('',*,*,#657,.F.);
#906=ORIENTED_EDGE('',*,*,#674,.T.);
#907=ORIENTED_EDGE('',*,*,#675,.F.);
#908=ORIENTED_EDGE('',*,*,#676,.F.);
#909=ORIENTED_EDGE('',*,*,#658,.F.);
#910=ORIENTED_EDGE('',*,*,#676,.T.);
#911=ORIENTED_EDGE('',*,*,#677,.F.);
#912=ORIENTED_EDGE('',*,*,#678,.F.);
#913=ORIENTED_EDGE('',*,*,#659,.F.);
#914=ORIENTED_EDGE('',*,*,#678,.T.);
#915=ORIENTED_EDGE('',*,*,#679,.F.);
#916=ORIENTED_EDGE('',*,*,#660,.T.);
#917=ORIENTED_EDGE('',*,*,#650,.F.);
#918=ORIENTED_EDGE('',*,*,#679,.T.);
#919=ORIENTED_EDGE('',*,*,#677,.T.);
#920=ORIENTED_EDGE('',*,*,#675,.T.);
#921=ORIENTED_EDGE('',*,*,#673,.T.);
#922=ORIENTED_EDGE('',*,*,#671,.T.);
#923=ORIENTED_EDGE('',*,*,#669,.T.);
#924=ORIENTED_EDGE('',*,*,#667,.T.);
#925=ORIENTED_EDGE('',*,*,#665,.T.);
#926=ORIENTED_EDGE('',*,*,#663,.T.);
#927=ORIENTED_EDGE('',*,*,#661,.T.);
#928=ORIENTED_EDGE('',*,*,#680,.T.);
#929=ORIENTED_EDGE('',*,*,#681,.T.);
#930=ORIENTED_EDGE('',*,*,#682,.T.);
#931=ORIENTED_EDGE('',*,*,#681,.F.);
#932=ORIENTED_EDGE('',*,*,#683,.T.);
#933=ORIENTED_EDGE('',*,*,#680,.F.);
#934=ORIENTED_EDGE('',*,*,#684,.T.);
#935=ORIENTED_EDGE('',*,*,#685,.T.);
#936=ORIENTED_EDGE('',*,*,#684,.F.);
#937=ORIENTED_EDGE('',*,*,#683,.F.);
#938=ORIENTED_EDGE('',*,*,#682,.F.);
#939=ORIENTED_EDGE('',*,*,#685,.F.);
#940=ORIENTED_EDGE('',*,*,#686,.F.);
#941=ORIENTED_EDGE('',*,*,#687,.F.);
#942=ORIENTED_EDGE('',*,*,#688,.T.);
#943=ORIENTED_EDGE('',*,*,#689,.F.);
#944=ORIENTED_EDGE('',*,*,#690,.F.);
#945=ORIENTED_EDGE('',*,*,#688,.F.);
#946=ORIENTED_EDGE('',*,*,#691,.F.);
#947=ORIENTED_EDGE('',*,*,#692,.F.);
#948=ORIENTED_EDGE('',*,*,#693,.F.);
#949=ORIENTED_EDGE('',*,*,#694,.T.);
#950=ORIENTED_EDGE('',*,*,#695,.F.);
#951=ORIENTED_EDGE('',*,*,#696,.F.);
#952=ORIENTED_EDGE('',*,*,#697,.F.);
#953=ORIENTED_EDGE('',*,*,#698,.F.);
#954=ORIENTED_EDGE('',*,*,#694,.F.);
#955=ORIENTED_EDGE('',*,*,#699,.F.);
#956=ORIENTED_EDGE('',*,*,#700,.F.);
#957=ORIENTED_EDGE('',*,*,#701,.T.);
#958=ORIENTED_EDGE('',*,*,#702,.F.);
#959=ORIENTED_EDGE('',*,*,#701,.F.);
#960=ORIENTED_EDGE('',*,*,#703,.F.);
#961=ORIENTED_EDGE('',*,*,#704,.F.);
#962=ORIENTED_EDGE('',*,*,#705,.F.);
#963=ORIENTED_EDGE('',*,*,#706,.F.);
#964=ORIENTED_EDGE('',*,*,#707,.F.);
#965=ORIENTED_EDGE('',*,*,#704,.T.);
#966=ORIENTED_EDGE('',*,*,#708,.F.);
#967=ORIENTED_EDGE('',*,*,#709,.F.);
#968=ORIENTED_EDGE('',*,*,#710,.T.);
#969=ORIENTED_EDGE('',*,*,#711,.T.);
#970=ORIENTED_EDGE('',*,*,#711,.F.);
#971=ORIENTED_EDGE('',*,*,#712,.T.);
#972=ORIENTED_EDGE('',*,*,#708,.T.);
#973=ORIENTED_EDGE('',*,*,#703,.T.);
#974=ORIENTED_EDGE('',*,*,#713,.T.);
#975=ORIENTED_EDGE('',*,*,#692,.T.);
#976=ORIENTED_EDGE('',*,*,#691,.T.);
#977=ORIENTED_EDGE('',*,*,#714,.T.);
#978=ORIENTED_EDGE('',*,*,#715,.F.);
#979=ORIENTED_EDGE('',*,*,#714,.F.);
#980=ORIENTED_EDGE('',*,*,#699,.T.);
#981=ORIENTED_EDGE('',*,*,#693,.T.);
#982=ORIENTED_EDGE('',*,*,#713,.F.);
#983=ORIENTED_EDGE('',*,*,#709,.T.);
#984=ORIENTED_EDGE('',*,*,#712,.F.);
#985=ORIENTED_EDGE('',*,*,#689,.T.);
#986=ORIENTED_EDGE('',*,*,#690,.T.);
#987=ORIENTED_EDGE('',*,*,#700,.T.);
#988=ORIENTED_EDGE('',*,*,#716,.F.);
#989=ORIENTED_EDGE('',*,*,#717,.T.);
#990=ORIENTED_EDGE('',*,*,#697,.T.);
#991=ORIENTED_EDGE('',*,*,#696,.T.);
#992=ORIENTED_EDGE('',*,*,#718,.T.);
#993=ORIENTED_EDGE('',*,*,#705,.T.);
#994=ORIENTED_EDGE('',*,*,#707,.T.);
#995=ORIENTED_EDGE('',*,*,#719,.T.);
#996=ORIENTED_EDGE('',*,*,#710,.F.);
#997=ORIENTED_EDGE('',*,*,#719,.F.);
#998=ORIENTED_EDGE('',*,*,#706,.T.);
#999=ORIENTED_EDGE('',*,*,#718,.F.);
#1000=ORIENTED_EDGE('',*,*,#695,.T.);
#1001=ORIENTED_EDGE('',*,*,#698,.T.);
#1002=ORIENTED_EDGE('',*,*,#717,.F.);
#1003=ORIENTED_EDGE('',*,*,#686,.T.);
#1004=ORIENTED_EDGE('',*,*,#687,.T.);
#1005=ORIENTED_EDGE('',*,*,#702,.T.);
#1006=ORIENTED_EDGE('',*,*,#716,.T.);
#1007=ORIENTED_EDGE('',*,*,#715,.T.);
#1008=CYLINDRICAL_SURFACE('',#1192,3.99999999999999);
#1009=CYLINDRICAL_SURFACE('',#1193,3.99999999999999);
#1010=CYLINDRICAL_SURFACE('',#1194,18.);
#1011=CYLINDRICAL_SURFACE('',#1197,20.);
#1012=CYLINDRICAL_SURFACE('',#1205,20.);
#1013=CYLINDRICAL_SURFACE('',#1207,24.);
#1014=CYLINDRICAL_SURFACE('',#1226,3.99999999999999);
#1015=CYLINDRICAL_SURFACE('',#1235,3.99999999999999);
#1016=CYLINDRICAL_SURFACE('',#1244,3.99999999999999);
#1017=CYLINDRICAL_SURFACE('',#1262,3.99999999999999);
#1018=CYLINDRICAL_SURFACE('',#1267,3.99999999999999);
#1019=CYLINDRICAL_SURFACE('',#1268,3.99999999999999);
#1020=CYLINDRICAL_SURFACE('',#1272,20.);
#1021=CYLINDRICAL_SURFACE('',#1274,22.);
#1022=ADVANCED_FACE('',(#171),#1008,.F.);
#1023=ADVANCED_FACE('',(#172),#1009,.F.);
#1024=ADVANCED_FACE('',(#173,#128),#1010,.F.);
#1025=ADVANCED_FACE('',(#174,#129),#1011,.T.);
#1026=ADVANCED_FACE('',(#175,#130),#97,.T.);
#1027=ADVANCED_FACE('',(#176,#131),#98,.F.);
#1028=ADVANCED_FACE('',(#177),#99,.F.);
#1029=ADVANCED_FACE('',(#178),#1012,.F.);
#1030=ADVANCED_FACE('',(#179),#1013,.T.);
#1031=ADVANCED_FACE('',(#180),#100,.T.);
#1032=ADVANCED_FACE('',(#181,#132),#101,.F.);
#1033=ADVANCED_FACE('',(#182),#102,.T.);
#1034=ADVANCED_FACE('',(#183),#103,.T.);
#1035=ADVANCED_FACE('',(#184),#104,.T.);
#1036=ADVANCED_FACE('',(#185),#51,.T.);
#1037=ADVANCED_FACE('',(#186),#52,.T.);
#1038=ADVANCED_FACE('',(#187),#105,.T.);
#1039=ADVANCED_FACE('',(#188),#106,.F.);
#1040=ADVANCED_FACE('',(#189),#53,.T.);
#1041=ADVANCED_FACE('',(#190),#107,.T.);
#1042=ADVANCED_FACE('',(#191),#108,.T.);
#1043=ADVANCED_FACE('',(#192),#109,.T.);
#1044=ADVANCED_FACE('',(#193),#54,.T.);
#1045=ADVANCED_FACE('',(#194),#47,.F.);
#1046=ADVANCED_FACE('',(#195),#1014,.T.);
#1047=ADVANCED_FACE('',(#196),#110,.F.);
#1048=ADVANCED_FACE('',(#197),#111,.T.);
#1049=ADVANCED_FACE('',(#198),#48,.F.);
#1050=ADVANCED_FACE('',(#199),#1015,.T.);
#1051=ADVANCED_FACE('',(#200),#112,.F.);
#1052=ADVANCED_FACE('',(#201),#113,.T.);
#1053=ADVANCED_FACE('',(#202),#49,.F.);
#1054=ADVANCED_FACE('',(#203),#1016,.T.);
#1055=ADVANCED_FACE('',(#204),#114,.T.);
#1056=ADVANCED_FACE('',(#205),#115,.F.);
#1057=ADVANCED_FACE('',(#206),#116,.F.);
#1058=ADVANCED_FACE('',(#207),#55,.T.);
#1059=ADVANCED_FACE('',(#208),#56,.T.);
#1060=ADVANCED_FACE('',(#209),#117,.T.);
#1061=ADVANCED_FACE('',(#210),#118,.T.);
#1062=ADVANCED_FACE('',(#211),#119,.T.);
#1063=ADVANCED_FACE('',(#212),#57,.T.);
#1064=ADVANCED_FACE('',(#213),#58,.T.);
#1065=ADVANCED_FACE('',(#214),#120,.T.);
#1066=ADVANCED_FACE('',(#215),#121,.T.);
#1067=ADVANCED_FACE('',(#216),#122,.T.);
#1068=ADVANCED_FACE('',(#217),#123,.T.);
#1069=ADVANCED_FACE('',(#218),#50,.F.);
#1070=ADVANCED_FACE('',(#219),#1017,.T.);
#1071=ADVANCED_FACE('',(#220),#124,.T.);
#1072=ADVANCED_FACE('',(#221),#125,.F.);
#1073=ADVANCED_FACE('',(#222),#1018,.F.);
#1074=ADVANCED_FACE('',(#223),#1019,.F.);
#1075=ADVANCED_FACE('',(#224),#59,.F.);
#1076=ADVANCED_FACE('',(#225),#60,.F.);
#1077=ADVANCED_FACE('',(#226,#133),#126,.F.);
#1078=ADVANCED_FACE('',(#227,#134,#135),#1020,.F.);
#1079=ADVANCED_FACE('',(#228,#136,#137),#1021,.T.);
#1080=ADVANCED_FACE('',(#229,#138),#127,.T.);
#1081=CLOSED_SHELL('',(#1022,#1023,#1024,#1025,#1026,#1027));
#1082=CLOSED_SHELL('',(#1028,#1029,#1030,#1031,#1032));
#1083=CLOSED_SHELL('',(#1033,#1034,#1035,#1036,#1037,#1038,#1039,#1040,
#1041,#1042,#1043,#1044));
#1084=CLOSED_SHELL('',(#1045,#1046,#1047,#1048));
#1085=CLOSED_SHELL('',(#1049,#1050,#1051,#1052));
#1086=CLOSED_SHELL('',(#1053,#1054,#1055,#1056));
#1087=CLOSED_SHELL('',(#1057,#1058,#1059,#1060,#1061,#1062,#1063,#1064,
#1065,#1066,#1067,#1068));
#1088=CLOSED_SHELL('',(#1069,#1070,#1071,#1072));
#1089=CLOSED_SHELL('',(#1073,#1074,#1075,#1076,#1077,#1078,#1079,#1080));
#1090=DERIVED_UNIT_ELEMENT(#1108,1.);
#1091=DERIVED_UNIT_ELEMENT(#3156,-3.);
#1092=DERIVED_UNIT_ELEMENT(#1108,1.);
#1093=DERIVED_UNIT_ELEMENT(#3156,-3.);
#1094=DERIVED_UNIT_ELEMENT(#1108,1.);
#1095=DERIVED_UNIT_ELEMENT(#3156,-3.);
#1096=DERIVED_UNIT_ELEMENT(#1108,1.);
#1097=DERIVED_UNIT_ELEMENT(#3156,-3.);
#1098=DERIVED_UNIT_ELEMENT(#1108,1.);
#1099=DERIVED_UNIT_ELEMENT(#3156,-3.);
#1100=DERIVED_UNIT_ELEMENT(#1108,1.);
#1101=DERIVED_UNIT_ELEMENT(#3156,-3.);
#1102=DERIVED_UNIT_ELEMENT(#1108,1.);
#1103=DERIVED_UNIT_ELEMENT(#3156,-3.);
#1104=DERIVED_UNIT_ELEMENT(#1108,1.);
#1105=DERIVED_UNIT_ELEMENT(#3156,-3.);
#1106=DERIVED_UNIT_ELEMENT(#1108,1.);
#1107=DERIVED_UNIT_ELEMENT(#3156,-3.);
#1108=(
MASS_UNIT()
NAMED_UNIT(*)
SI_UNIT(.KILO.,.GRAM.)
);
#1109=DERIVED_UNIT((#1090,#1091));
#1110=DERIVED_UNIT((#1092,#1093));
#1111=DERIVED_UNIT((#1094,#1095));
#1112=DERIVED_UNIT((#1096,#1097));
#1113=DERIVED_UNIT((#1098,#1099));
#1114=DERIVED_UNIT((#1100,#1101));
#1115=DERIVED_UNIT((#1102,#1103));
#1116=DERIVED_UNIT((#1104,#1105));
#1117=DERIVED_UNIT((#1106,#1107));
#1118=MEASURE_REPRESENTATION_ITEM('density measure',
POSITIVE_RATIO_MEASURE(7850.),#1109);
#1119=MEASURE_REPRESENTATION_ITEM('density measure',
POSITIVE_RATIO_MEASURE(7850.),#1110);
#1120=MEASURE_REPRESENTATION_ITEM('density measure',
POSITIVE_RATIO_MEASURE(7850.),#1111);
#1121=MEASURE_REPRESENTATION_ITEM('density measure',
POSITIVE_RATIO_MEASURE(7850.),#1112);
#1122=MEASURE_REPRESENTATION_ITEM('density measure',
POSITIVE_RATIO_MEASURE(7850.),#1113);
#1123=MEASURE_REPRESENTATION_ITEM('density measure',
POSITIVE_RATIO_MEASURE(7850.),#1114);
#1124=MEASURE_REPRESENTATION_ITEM('density measure',
POSITIVE_RATIO_MEASURE(7850.),#1115);
#1125=MEASURE_REPRESENTATION_ITEM('density measure',
POSITIVE_RATIO_MEASURE(7850.),#1116);
#1126=MEASURE_REPRESENTATION_ITEM('density measure',
POSITIVE_RATIO_MEASURE(7850.),#1117);
#1127=PROPERTY_DEFINITION_REPRESENTATION(#1172,#1145);
#1128=PROPERTY_DEFINITION_REPRESENTATION(#1173,#1146);
#1129=PROPERTY_DEFINITION_REPRESENTATION(#1174,#1147);
#1130=PROPERTY_DEFINITION_REPRESENTATION(#1175,#1148);
#1131=PROPERTY_DEFINITION_REPRESENTATION(#1176,#1149);
#1132=PROPERTY_DEFINITION_REPRESENTATION(#1177,#1150);
#1133=PROPERTY_DEFINITION_REPRESENTATION(#1178,#1151);
#1134=PROPERTY_DEFINITION_REPRESENTATION(#1179,#1152);
#1135=PROPERTY_DEFINITION_REPRESENTATION(#1180,#1153);
#1136=PROPERTY_DEFINITION_REPRESENTATION(#1181,#1154);
#1137=PROPERTY_DEFINITION_REPRESENTATION(#1182,#1155);
#1138=PROPERTY_DEFINITION_REPRESENTATION(#1183,#1156);
#1139=PROPERTY_DEFINITION_REPRESENTATION(#1184,#1157);
#1140=PROPERTY_DEFINITION_REPRESENTATION(#1185,#1158);
#1141=PROPERTY_DEFINITION_REPRESENTATION(#1186,#1159);
#1142=PROPERTY_DEFINITION_REPRESENTATION(#1187,#1160);
#1143=PROPERTY_DEFINITION_REPRESENTATION(#1188,#1161);
#1144=PROPERTY_DEFINITION_REPRESENTATION(#1189,#1162);
#1145=REPRESENTATION('material name',(#1163),#3145);
#1146=REPRESENTATION('density',(#1118),#3145);
#1147=REPRESENTATION('material name',(#1164),#3146);
#1148=REPRESENTATION('density',(#1119),#3146);
#1149=REPRESENTATION('material name',(#1165),#3147);
#1150=REPRESENTATION('density',(#1120),#3147);
#1151=REPRESENTATION('material name',(#1166),#3148);
#1152=REPRESENTATION('density',(#1121),#3148);
#1153=REPRESENTATION('material name',(#1167),#3149);
#1154=REPRESENTATION('density',(#1122),#3149);
#1155=REPRESENTATION('material name',(#1168),#3150);
#1156=REPRESENTATION('density',(#1123),#3150);
#1157=REPRESENTATION('material name',(#1169),#3151);
#1158=REPRESENTATION('density',(#1124),#3151);
#1159=REPRESENTATION('material name',(#1170),#3152);
#1160=REPRESENTATION('density',(#1125),#3152);
#1161=REPRESENTATION('material name',(#1171),#3153);
#1162=REPRESENTATION('density',(#1126),#3153);
#1163=DESCRIPTIVE_REPRESENTATION_ITEM('Steel','Steel');
#1164=DESCRIPTIVE_REPRESENTATION_ITEM('Steel','Steel');
#1165=DESCRIPTIVE_REPRESENTATION_ITEM('Steel','Steel');
#1166=DESCRIPTIVE_REPRESENTATION_ITEM('Steel','Steel');
#1167=DESCRIPTIVE_REPRESENTATION_ITEM('Steel','Steel');
#1168=DESCRIPTIVE_REPRESENTATION_ITEM('Steel','Steel');
#1169=DESCRIPTIVE_REPRESENTATION_ITEM('Steel','Steel');
#1170=DESCRIPTIVE_REPRESENTATION_ITEM('Steel','Steel');
#1171=DESCRIPTIVE_REPRESENTATION_ITEM('Steel','Steel');
#1172=PROPERTY_DEFINITION('material property','material name',#3200);
#1173=PROPERTY_DEFINITION('material property','density of part',#3200);
#1174=PROPERTY_DEFINITION('material property','material name',#3201);
#1175=PROPERTY_DEFINITION('material property','density of part',#3201);
#1176=PROPERTY_DEFINITION('material property','material name',#3202);
#1177=PROPERTY_DEFINITION('material property','density of part',#3202);
#1178=PROPERTY_DEFINITION('material property','material name',#3203);
#1179=PROPERTY_DEFINITION('material property','density of part',#3203);
#1180=PROPERTY_DEFINITION('material property','material name',#3204);
#1181=PROPERTY_DEFINITION('material property','density of part',#3204);
#1182=PROPERTY_DEFINITION('material property','material name',#3205);
#1183=PROPERTY_DEFINITION('material property','density of part',#3205);
#1184=PROPERTY_DEFINITION('material property','material name',#3206);
#1185=PROPERTY_DEFINITION('material property','density of part',#3206);
#1186=PROPERTY_DEFINITION('material property','material name',#3207);
#1187=PROPERTY_DEFINITION('material property','density of part',#3207);
#1188=PROPERTY_DEFINITION('material property','material name',#3208);
#1189=PROPERTY_DEFINITION('material property','density of part',#3208);
#1190=AXIS2_PLACEMENT_3D('',#1544,#1286,#1287);
#1191=AXIS2_PLACEMENT_3D('',#1545,#1288,#1289);
#1192=AXIS2_PLACEMENT_3D('',#1546,#1290,#1291);
#1193=AXIS2_PLACEMENT_3D('',#1632,#1293,#1294);
#1194=AXIS2_PLACEMENT_3D('',#1710,#1296,#1297);
#1195=AXIS2_PLACEMENT_3D('',#1712,#1298,#1299);
#1196=AXIS2_PLACEMENT_3D('',#1716,#1302,#1303);
#1197=AXIS2_PLACEMENT_3D('',#1717,#1304,#1305);
#1198=AXIS2_PLACEMENT_3D('',#1719,#1306,#1307);
#1199=AXIS2_PLACEMENT_3D('',#1723,#1310,#1311);
#1200=AXIS2_PLACEMENT_3D('',#1724,#1312,#1313);
#1201=AXIS2_PLACEMENT_3D('',#1725,#1314,#1315);
#1202=AXIS2_PLACEMENT_3D('',#1726,#1316,#1317);
#1203=AXIS2_PLACEMENT_3D('',#1727,#1318,#1319);
#1204=AXIS2_PLACEMENT_3D('',#1729,#1320,#1321);
#1205=AXIS2_PLACEMENT_3D('',#1730,#1322,#1323);
#1206=AXIS2_PLACEMENT_3D('',#1733,#1325,#1326);
#1207=AXIS2_PLACEMENT_3D('',#1734,#1327,#1328);
#1208=AXIS2_PLACEMENT_3D('',#1736,#1329,#1330);
#1209=AXIS2_PLACEMENT_3D('',#1739,#1332,#1333);
#1210=AXIS2_PLACEMENT_3D('',#1740,#1334,#1335);
#1211=AXIS2_PLACEMENT_3D('',#1741,#1336,#1337);
#1212=AXIS2_PLACEMENT_3D('',#1742,#1338,#1339);
#1213=AXIS2_PLACEMENT_3D('',#1743,#1340,#1341);
#1214=AXIS2_PLACEMENT_3D('',#1752,#1346,#1347);
#1215=AXIS2_PLACEMENT_3D('',#1758,#1351,#1352);
#1216=AXIS2_PLACEMENT_3D('',#1944,#1358,#1359);
#1217=AXIS2_PLACEMENT_3D('',#1995,#1363,#1364);
#1218=AXIS2_PLACEMENT_3D('',#2097,#1369,#1370);
#1219=AXIS2_PLACEMENT_3D('',#2099,#1372,#1373);
#1220=AXIS2_PLACEMENT_3D('',#2101,#1375,#1376);
#1221=AXIS2_PLACEMENT_3D('',#2141,#1378,#1379);
#1222=AXIS2_PLACEMENT_3D('',#2171,#1380,#1381);
#1223=AXIS2_PLACEMENT_3D('',#2172,#1382,#1383);
#1224=AXIS2_PLACEMENT_3D('',#2174,#1384,#1385);
#1225=AXIS2_PLACEMENT_3D('',#2175,#1386,#1387);
#1226=AXIS2_PLACEMENT_3D('',#2176,#1388,#1389);
#1227=AXIS2_PLACEMENT_3D('',#2178,#1390,#1391);
#1228=AXIS2_PLACEMENT_3D('',#2180,#1393,#1394);
#1229=AXIS2_PLACEMENT_3D('',#2181,#1395,#1396);
#1230=AXIS2_PLACEMENT_3D('',#2182,#1397,#1398);
#1231=AXIS2_PLACEMENT_3D('',#2212,#1399,#1400);
#1232=AXIS2_PLACEMENT_3D('',#2213,#1401,#1402);
#1233=AXIS2_PLACEMENT_3D('',#2215,#1403,#1404);
#1234=AXIS2_PLACEMENT_3D('',#2216,#1405,#1406);
#1235=AXIS2_PLACEMENT_3D('',#2217,#1407,#1408);
#1236=AXIS2_PLACEMENT_3D('',#2219,#1409,#1410);
#1237=AXIS2_PLACEMENT_3D('',#2221,#1412,#1413);
#1238=AXIS2_PLACEMENT_3D('',#2222,#1414,#1415);
#1239=AXIS2_PLACEMENT_3D('',#2223,#1416,#1417);
#1240=AXIS2_PLACEMENT_3D('',#2253,#1418,#1419);
#1241=AXIS2_PLACEMENT_3D('',#2255,#1420,#1421);
#1242=AXIS2_PLACEMENT_3D('',#2256,#1422,#1423);
#1243=AXIS2_PLACEMENT_3D('',#2257,#1424,#1425);
#1244=AXIS2_PLACEMENT_3D('',#2258,#1426,#1427);
#1245=AXIS2_PLACEMENT_3D('',#2261,#1429,#1430);
#1246=AXIS2_PLACEMENT_3D('',#2262,#1431,#1432);
#1247=AXIS2_PLACEMENT_3D('',#2263,#1433,#1434);
#1248=AXIS2_PLACEMENT_3D('',#2264,#1435,#1436);
#1249=AXIS2_PLACEMENT_3D('',#2265,#1437,#1438);
#1250=AXIS2_PLACEMENT_3D('',#2468,#1448,#1449);
#1251=AXIS2_PLACEMENT_3D('',#2472,#1452,#1453);
#1252=AXIS2_PLACEMENT_3D('',#2476,#1456,#1457);
#1253=AXIS2_PLACEMENT_3D('',#2556,#1462,#1463);
#1254=AXIS2_PLACEMENT_3D('',#2560,#1466,#1467);
#1255=AXIS2_PLACEMENT_3D('',#2564,#1470,#1471);
#1256=AXIS2_PLACEMENT_3D('',#2566,#1473,#1474);
#1257=AXIS2_PLACEMENT_3D('',#2567,#1475,#1476);
#1258=AXIS2_PLACEMENT_3D('',#2597,#1477,#1478);
#1259=AXIS2_PLACEMENT_3D('',#2599,#1479,#1480);
#1260=AXIS2_PLACEMENT_3D('',#2600,#1481,#1482);
#1261=AXIS2_PLACEMENT_3D('',#2601,#1483,#1484);
#1262=AXIS2_PLACEMENT_3D('',#2602,#1485,#1486);
#1263=AXIS2_PLACEMENT_3D('',#2605,#1488,#1489);
#1264=AXIS2_PLACEMENT_3D('',#2606,#1490,#1491);
#1265=AXIS2_PLACEMENT_3D('',#2607,#1492,#1493);
#1266=AXIS2_PLACEMENT_3D('',#2608,#1494,#1495);
#1267=AXIS2_PLACEMENT_3D('',#2609,#1496,#1497);
#1268=AXIS2_PLACEMENT_3D('',#2687,#1499,#1500);
#1269=AXIS2_PLACEMENT_3D('',#3106,#1504,#1505);
#1270=AXIS2_PLACEMENT_3D('',#3108,#1506,#1507);
#1271=AXIS2_PLACEMENT_3D('',#3110,#1508,#1509);
#1272=AXIS2_PLACEMENT_3D('',#3111,#1510,#1511);
#1273=AXIS2_PLACEMENT_3D('',#3116,#1515,#1516);
#1274=AXIS2_PLACEMENT_3D('',#3117,#1517,#1518);
#1275=AXIS2_PLACEMENT_3D('',#3119,#1519,#1520);
#1276=AXIS2_PLACEMENT_3D('',#3123,#1524,#1525);
#1277=AXIS2_PLACEMENT_3D('',#3124,#1526,#1527);
#1278=AXIS2_PLACEMENT_3D('',#3125,#1528,#1529);
#1279=AXIS2_PLACEMENT_3D('',#3126,#1530,#1531);
#1280=AXIS2_PLACEMENT_3D('',#3127,#1532,#1533);
#1281=AXIS2_PLACEMENT_3D('',#3128,#1534,#1535);
#1282=AXIS2_PLACEMENT_3D('',#3129,#1536,#1537);
#1283=AXIS2_PLACEMENT_3D('',#3130,#1538,#1539);
#1284=AXIS2_PLACEMENT_3D('',#3131,#1540,#1541);
#1285=AXIS2_PLACEMENT_3D('',#3132,#1542,#1543);
#1286=DIRECTION('axis',(0.,0.,1.));
#1287=DIRECTION('refdir',(1.,0.,0.));
#1288=DIRECTION('axis',(0.,0.,1.));
#1289=DIRECTION('refdir',(1.,0.,0.));
#1290=DIRECTION('center_axis',(1.,0.,0.));
#1291=DIRECTION('ref_axis',(0.,1.,0.));
#1292=DIRECTION('',(1.,0.,0.));
#1293=DIRECTION('center_axis',(1.,0.,0.));
#1294=DIRECTION('ref_axis',(0.,1.,0.));
#1295=DIRECTION('',(1.,0.,0.));
#1296=DIRECTION('center_axis',(0.,0.,1.));
#1297=DIRECTION('ref_axis',(1.,0.,0.));
#1298=DIRECTION('center_axis',(0.,0.,-1.));
#1299=DIRECTION('ref_axis',(1.,0.,0.));
#1300=DIRECTION('',(0.,0.,1.));
#1301=DIRECTION('',(0.,0.,1.));
#1302=DIRECTION('center_axis',(0.,0.,-1.));
#1303=DIRECTION('ref_axis',(1.,0.,0.));
#1304=DIRECTION('center_axis',(0.,0.,1.));
#1305=DIRECTION('ref_axis',(1.,0.,0.));
#1306=DIRECTION('center_axis',(0.,0.,1.));
#1307=DIRECTION('ref_axis',(1.,0.,0.));
#1308=DIRECTION('',(0.,0.,-1.));
#1309=DIRECTION('',(0.,0.,-1.));
#1310=DIRECTION('center_axis',(0.,0.,1.));
#1311=DIRECTION('ref_axis',(1.,0.,0.));
#1312=DIRECTION('center_axis',(0.,0.,1.));
#1313=DIRECTION('ref_axis',(1.,0.,0.));
#1314=DIRECTION('center_axis',(0.,0.,1.));
#1315=DIRECTION('ref_axis',(1.,0.,0.));
#1316=DIRECTION('axis',(0.,0.,1.));
#1317=DIRECTION('refdir',(1.,0.,0.));
#1318=DIRECTION('center_axis',(0.,0.,-1.));
#1319=DIRECTION('ref_axis',(1.,0.,0.));
#1320=DIRECTION('center_axis',(0.,0.,-1.));
#1321=DIRECTION('ref_axis',(1.,0.,0.));
#1322=DIRECTION('center_axis',(0.,0.,1.));
#1323=DIRECTION('ref_axis',(1.,0.,0.));
#1324=DIRECTION('',(0.,0.,1.));
#1325=DIRECTION('center_axis',(0.,0.,-1.));
#1326=DIRECTION('ref_axis',(1.,0.,0.));
#1327=DIRECTION('center_axis',(0.,0.,1.));
#1328=DIRECTION('ref_axis',(1.,0.,0.));
#1329=DIRECTION('center_axis',(0.,0.,1.));
#1330=DIRECTION('ref_axis',(1.,0.,0.));
#1331=DIRECTION('',(0.,0.,-1.));
#1332=DIRECTION('center_axis',(0.,0.,-1.));
#1333=DIRECTION('ref_axis',(1.,0.,0.));
#1334=DIRECTION('center_axis',(0.,0.,-1.));
#1335=DIRECTION('ref_axis',(1.,0.,0.));
#1336=DIRECTION('center_axis',(0.,0.,-1.));
#1337=DIRECTION('ref_axis',(1.,0.,0.));
#1338=DIRECTION('axis',(0.,0.,1.));
#1339=DIRECTION('refdir',(1.,0.,0.));
#1340=DIRECTION('center_axis',(-1.,0.,0.));
#1341=DIRECTION('ref_axis',(0.,0.,1.));
#1342=DIRECTION('',(0.,1.,0.));
#1343=DIRECTION('',(0.,0.,1.));
#1344=DIRECTION('',(0.,-1.,0.));
#1345=DIRECTION('',(0.,0.,-1.));
#1346=DIRECTION('center_axis',(0.,0.,1.));
#1347=DIRECTION('ref_axis',(1.,0.,0.));
#1348=DIRECTION('',(0.,1.,0.));
#1349=DIRECTION('',(1.,0.,0.));
#1350=DIRECTION('',(-1.,0.,0.));
#1351=DIRECTION('center_axis',(1.,0.,0.));
#1352=DIRECTION('ref_axis',(0.,0.,-1.));
#1353=DIRECTION('',(0.,1.,0.));
#1354=DIRECTION('',(0.,0.,-1.));
#1355=DIRECTION('',(0.,0.,1.));
#1356=DIRECTION('',(0.,-1.,0.));
#1357=DIRECTION('',(0.,-1.,0.));
#1358=DIRECTION('center_axis',(0.,1.,0.));
#1359=DIRECTION('ref_axis',(1.,0.,0.));
#1360=DIRECTION('',(0.,0.,1.));
#1361=DIRECTION('',(1.,0.,0.));
#1362=DIRECTION('',(0.,0.,-1.));
#1363=DIRECTION('center_axis',(0.,1.,0.));
#1364=DIRECTION('ref_axis',(1.,0.,0.));
#1365=DIRECTION('',(0.,0.,1.));
#1366=DIRECTION('',(-1.,0.,0.));
#1367=DIRECTION('',(0.,0.,-1.));
#1368=DIRECTION('',(0.,1.,0.));
#1369=DIRECTION('center_axis',(1.,0.,0.));
#1370=DIRECTION('ref_axis',(0.,0.,-1.));
#1371=DIRECTION('',(0.,1.,0.));
#1372=DIRECTION('center_axis',(0.,0.,1.));
#1373=DIRECTION('ref_axis',(1.,0.,0.));
#1374=DIRECTION('',(0.,1.,0.));
#1375=DIRECTION('center_axis',(-1.,0.,0.));
#1376=DIRECTION('ref_axis',(0.,0.,1.));
#1377=DIRECTION('',(0.,1.,0.));
#1378=DIRECTION('axis',(0.,0.,1.));
#1379=DIRECTION('refdir',(1.,0.,0.));
#1380=DIRECTION('center_axis',(1.,0.,0.));
#1381=DIRECTION('ref_axis',(0.,1.,0.));
#1382=DIRECTION('center_axis',(1.,0.,0.));
#1383=DIRECTION('ref_axis',(0.,1.,0.));
#1384=DIRECTION('center_axis',(-5.11592739497909E-14,-1.,-1.22464679913998E-16));
#1385=DIRECTION('ref_axis',(1.44328993201271E-14,-1.22464679914736E-16,
1.));
#1386=DIRECTION('center_axis',(-1.,0.,0.));
#1387=DIRECTION('ref_axis',(0.,1.,0.));
#1388=DIRECTION('center_axis',(1.,0.,0.));
#1389=DIRECTION('ref_axis',(0.,1.,0.));
#1390=DIRECTION('center_axis',(1.,0.,0.));
#1391=DIRECTION('ref_axis',(0.,1.,0.));
#1392=DIRECTION('',(-1.,0.,0.));
#1393=DIRECTION('center_axis',(1.,0.,0.));
#1394=DIRECTION('ref_axis',(0.,1.,0.));
#1395=DIRECTION('center_axis',(1.,0.,0.));
#1396=DIRECTION('ref_axis',(0.,1.,0.));
#1397=DIRECTION('axis',(0.,0.,1.));
#1398=DIRECTION('refdir',(1.,0.,0.));
#1399=DIRECTION('center_axis',(1.,0.,0.));
#1400=DIRECTION('ref_axis',(0.,1.,0.));
#1401=DIRECTION('center_axis',(1.,0.,0.));
#1402=DIRECTION('ref_axis',(0.,1.,0.));
#1403=DIRECTION('center_axis',(-3.42164774028179E-14,-1.,-1.22464679909721E-16));
#1404=DIRECTION('ref_axis',(1.46549439250521E-13,-1.22464679914735E-16,
1.));
#1405=DIRECTION('center_axis',(-1.,0.,0.));
#1406=DIRECTION('ref_axis',(0.,1.,0.));
#1407=DIRECTION('center_axis',(1.,0.,0.));
#1408=DIRECTION('ref_axis',(0.,1.,0.));
#1409=DIRECTION('center_axis',(1.,0.,0.));
#1410=DIRECTION('ref_axis',(0.,1.,0.));
#1411=DIRECTION('',(-1.,0.,0.));
#1412=DIRECTION('center_axis',(1.,0.,0.));
#1413=DIRECTION('ref_axis',(0.,1.,0.));
#1414=DIRECTION('center_axis',(1.,0.,0.));
#1415=DIRECTION('ref_axis',(0.,1.,0.));
#1416=DIRECTION('axis',(0.,0.,1.));
#1417=DIRECTION('refdir',(1.,0.,0.));
#1418=DIRECTION('center_axis',(1.,0.,0.));
#1419=DIRECTION('ref_axis',(0.,1.,0.));
#1420=DIRECTION('center_axis',(-5.11592739497909E-14,1.,1.22464679913998E-16));
#1421=DIRECTION('ref_axis',(-1.44328993201271E-14,-1.22464679914736E-16,
1.));
#1422=DIRECTION('center_axis',(-1.,0.,0.));
#1423=DIRECTION('ref_axis',(0.,1.,0.));
#1424=DIRECTION('center_axis',(1.,0.,0.));
#1425=DIRECTION('ref_axis',(0.,1.,0.));
#1426=DIRECTION('center_axis',(1.,0.,0.));
#1427=DIRECTION('ref_axis',(0.,1.,0.));
#1428=DIRECTION('',(-1.,0.,0.));
#1429=DIRECTION('center_axis',(1.,0.,0.));
#1430=DIRECTION('ref_axis',(0.,1.,0.));
#1431=DIRECTION('center_axis',(1.,0.,0.));
#1432=DIRECTION('ref_axis',(0.,1.,0.));
#1433=DIRECTION('center_axis',(1.,0.,0.));
#1434=DIRECTION('ref_axis',(0.,1.,0.));
#1435=DIRECTION('axis',(0.,0.,1.));
#1436=DIRECTION('refdir',(1.,0.,0.));
#1437=DIRECTION('center_axis',(0.,1.,0.));
#1438=DIRECTION('ref_axis',(1.,0.,0.));
#1439=DIRECTION('',(0.,0.,-1.));
#1440=DIRECTION('',(0.,0.,1.));
#1441=DIRECTION('',(-1.,0.,0.));
#1442=DIRECTION('',(0.,0.,-1.));
#1443=DIRECTION('',(0.,0.,1.));
#1444=DIRECTION('',(-1.,0.,0.));
#1445=DIRECTION('',(0.,-1.,0.));
#1446=DIRECTION('',(0.,1.,0.));
#1447=DIRECTION('',(0.,1.,0.));
#1448=DIRECTION('center_axis',(1.,0.,0.));
#1449=DIRECTION('ref_axis',(0.,0.,-1.));
#1450=DIRECTION('',(0.,0.,-1.));
#1451=DIRECTION('',(0.,1.,0.));
#1452=DIRECTION('center_axis',(0.,0.,1.));
#1453=DIRECTION('ref_axis',(1.,0.,0.));
#1454=DIRECTION('',(1.,0.,0.));
#1455=DIRECTION('',(0.,1.,0.));
#1456=DIRECTION('center_axis',(-1.,0.,0.));
#1457=DIRECTION('ref_axis',(0.,0.,1.));
#1458=DIRECTION('',(0.,0.,1.));
#1459=DIRECTION('',(0.,1.,0.));
#1460=DIRECTION('',(0.,1.,0.));
#1461=DIRECTION('',(0.,1.,0.));
#1462=DIRECTION('center_axis',(1.,0.,0.));
#1463=DIRECTION('ref_axis',(0.,0.,-1.));
#1464=DIRECTION('',(0.,0.,-1.));
#1465=DIRECTION('',(0.,1.,0.));
#1466=DIRECTION('center_axis',(0.,0.,1.));
#1467=DIRECTION('ref_axis',(1.,0.,0.));
#1468=DIRECTION('',(1.,0.,0.));
#1469=DIRECTION('',(0.,1.,0.));
#1470=DIRECTION('center_axis',(-1.,0.,0.));
#1471=DIRECTION('ref_axis',(0.,0.,1.));
#1472=DIRECTION('',(0.,0.,1.));
#1473=DIRECTION('center_axis',(0.,1.,0.));
#1474=DIRECTION('ref_axis',(1.,0.,0.));
#1475=DIRECTION('axis',(0.,0.,1.));
#1476=DIRECTION('refdir',(1.,0.,0.));
#1477=DIRECTION('center_axis',(1.,0.,0.));
#1478=DIRECTION('ref_axis',(0.,1.,0.));
#1479=DIRECTION('center_axis',(-3.42164774028179E-14,1.,1.22464679909721E-16));
#1480=DIRECTION('ref_axis',(-1.46549439250521E-13,-1.22464679914735E-16,
1.));
#1481=DIRECTION('center_axis',(-1.,0.,0.));
#1482=DIRECTION('ref_axis',(0.,1.,0.));
#1483=DIRECTION('center_axis',(1.,0.,0.));
#1484=DIRECTION('ref_axis',(0.,1.,0.));
#1485=DIRECTION('center_axis',(1.,0.,0.));
#1486=DIRECTION('ref_axis',(0.,1.,0.));
#1487=DIRECTION('',(-1.,0.,0.));
#1488=DIRECTION('center_axis',(1.,0.,0.));
#1489=DIRECTION('ref_axis',(0.,1.,0.));
#1490=DIRECTION('center_axis',(1.,0.,0.));
#1491=DIRECTION('ref_axis',(0.,1.,0.));
#1492=DIRECTION('center_axis',(1.,0.,0.));
#1493=DIRECTION('ref_axis',(0.,1.,0.));
#1494=DIRECTION('axis',(0.,0.,1.));
#1495=DIRECTION('refdir',(1.,0.,0.));
#1496=DIRECTION('center_axis',(1.,0.,0.));
#1497=DIRECTION('ref_axis',(0.,1.,0.));
#1498=DIRECTION('',(1.,0.,0.));
#1499=DIRECTION('center_axis',(1.,0.,0.));
#1500=DIRECTION('ref_axis',(0.,1.,0.));
#1501=DIRECTION('',(1.,0.,0.));
#1502=DIRECTION('',(-1.,0.,0.));
#1503=DIRECTION('',(-1.,0.,0.));
#1504=DIRECTION('center_axis',(0.,0.,1.));
#1505=DIRECTION('ref_axis',(-1.,0.,0.));
#1506=DIRECTION('center_axis',(0.,0.,-1.));
#1507=DIRECTION('ref_axis',(-1.,0.,0.));
#1508=DIRECTION('center_axis',(0.,0.,1.));
#1509=DIRECTION('ref_axis',(-1.,0.,0.));
#1510=DIRECTION('center_axis',(0.,0.,1.));
#1511=DIRECTION('ref_axis',(-1.,0.,0.));
#1512=DIRECTION('',(0.,0.,1.));
#1513=DIRECTION('',(0.,0.,1.));
#1514=DIRECTION('',(0.,0.,1.));
#1515=DIRECTION('center_axis',(0.,0.,-1.));
#1516=DIRECTION('ref_axis',(-1.,0.,0.));
#1517=DIRECTION('center_axis',(0.,0.,1.));
#1518=DIRECTION('ref_axis',(-1.,0.,0.));
#1519=DIRECTION('center_axis',(0.,0.,1.));
#1520=DIRECTION('ref_axis',(-1.,0.,0.));
#1521=DIRECTION('',(0.,0.,-1.));
#1522=DIRECTION('',(0.,0.,-1.));
#1523=DIRECTION('',(0.,0.,-1.));
#1524=DIRECTION('center_axis',(0.,0.,1.));
#1525=DIRECTION('ref_axis',(-1.,0.,0.));
#1526=DIRECTION('',(0.,0.,1.));
#1527=DIRECTION('',(1.,0.,0.));
#1528=DIRECTION('',(0.,0.,1.));
#1529=DIRECTION('',(1.,0.,0.));
#1530=DIRECTION('',(0.,0.,1.));
#1531=DIRECTION('',(1.,0.,0.));
#1532=DIRECTION('',(0.,0.,1.));
#1533=DIRECTION('',(1.,0.,0.));
#1534=DIRECTION('',(0.,0.,1.));
#1535=DIRECTION('',(1.,0.,0.));
#1536=DIRECTION('',(0.,0.,1.));
#1537=DIRECTION('',(1.,0.,0.));
#1538=DIRECTION('',(0.,0.,1.));
#1539=DIRECTION('',(1.,0.,0.));
#1540=DIRECTION('',(0.,0.,1.));
#1541=DIRECTION('',(1.,0.,0.));
#1542=DIRECTION('',(0.,0.,1.));
#1543=DIRECTION('',(1.,0.,0.));
#1544=CARTESIAN_POINT('',(0.,0.,0.));
#1545=CARTESIAN_POINT('',(0.,0.,0.));
#1546=CARTESIAN_POINT('Origin',(0.,0.,180.));
#1547=CARTESIAN_POINT('',(-20.,-1.98792512857715E-15,176.));
#1548=CARTESIAN_POINT('',(-20.,-1.05117445154967E-15,184.));
#1549=CARTESIAN_POINT('Ctrl Pts',(-20.,-2.77555756156289E-16,184.));
#1550=CARTESIAN_POINT('Ctrl Pts',(-20.,0.503698781685596,184.));
#1551=CARTESIAN_POINT('Ctrl Pts',(-19.9790475458833,1.04005322432747,183.899058168943));
#1552=CARTESIAN_POINT('Ctrl Pts',(-19.9033338860745,2.02517944479051,183.490417366179));
#1553=CARTESIAN_POINT('Ctrl Pts',(-19.8496135055327,2.47406169858037,183.182792550912));
#1554=CARTESIAN_POINT('Ctrl Pts',(-19.7483634040773,3.18281240876835,182.474041840724));
#1555=CARTESIAN_POINT('Ctrl Pts',(-19.6941660317108,3.4904216705935,182.02516802012));
#1556=CARTESIAN_POINT('Ctrl Pts',(-19.6173550647379,3.89905118499443,181.040071108648));
#1557=CARTESIAN_POINT('Ctrl Pts',(-19.5959179422654,3.99999999999999,180.503727007854));
#1558=CARTESIAN_POINT('Ctrl Pts',(-19.5959179422654,3.99999999999999,180.));
#1559=CARTESIAN_POINT('Ctrl Pts',(-19.5959179422654,3.99999999999999,179.496272992146));
#1560=CARTESIAN_POINT('Ctrl Pts',(-19.6173550647379,3.89905118499443,178.959928891352));
#1561=CARTESIAN_POINT('Ctrl Pts',(-19.6941660317108,3.4904216705935,177.97483197988));
#1562=CARTESIAN_POINT('Ctrl Pts',(-19.7483634040773,3.18281240876835,177.525958159276));
#1563=CARTESIAN_POINT('Ctrl Pts',(-19.8496135055327,2.47406169858037,176.817207449088));
#1564=CARTESIAN_POINT('Ctrl Pts',(-19.9033338860745,2.02517944479051,176.509582633821));
#1565=CARTESIAN_POINT('Ctrl Pts',(-19.9790475458833,1.04005322432747,176.100941831057));
#1566=CARTESIAN_POINT('Ctrl Pts',(-20.,0.503698781685596,176.));
#1567=CARTESIAN_POINT('Ctrl Pts',(-20.,-1.2490009027033E-15,176.));
#1568=CARTESIAN_POINT('',(-19.5959179422654,-3.99999999999999,180.));
#1569=CARTESIAN_POINT('Ctrl Pts',(-20.,-9.71445146547012E-16,176.));
#1570=CARTESIAN_POINT('Ctrl Pts',(-20.,-0.503698781685598,176.));
#1571=CARTESIAN_POINT('Ctrl Pts',(-19.9790475458833,-1.04005322432746,176.100941831057));
#1572=CARTESIAN_POINT('Ctrl Pts',(-19.9033338860745,-2.0251794447905,176.509582633821));
#1573=CARTESIAN_POINT('Ctrl Pts',(-19.8496135055327,-2.47406169858037,176.817207449088));
#1574=CARTESIAN_POINT('Ctrl Pts',(-19.7483634040773,-3.18281240876835,177.525958159276));
#1575=CARTESIAN_POINT('Ctrl Pts',(-19.6941660317108,-3.4904216705935,177.97483197988));
#1576=CARTESIAN_POINT('Ctrl Pts',(-19.6173550647379,-3.89905118499443,178.959928891352));
#1577=CARTESIAN_POINT('Ctrl Pts',(-19.5959179422654,-3.99999999999999,179.496272992146));
#1578=CARTESIAN_POINT('Ctrl Pts',(-19.5959179422654,-3.99999999999999,180.));
#1579=CARTESIAN_POINT('',(-17.5499287747842,-3.99999999999999,180.));
#1580=CARTESIAN_POINT('',(0.,-3.99999999999999,180.));
#1581=CARTESIAN_POINT('',(-18.,-2.48996090001406E-15,176.));
#1582=CARTESIAN_POINT('Ctrl Pts',(-17.5499287747842,-3.99999999999999,180.));
#1583=CARTESIAN_POINT('Ctrl Pts',(-17.5499287747842,-3.99999999999999,179.495913499213));
#1584=CARTESIAN_POINT('Ctrl Pts',(-17.5739034455062,-3.89891257329756,178.959425202916));
#1585=CARTESIAN_POINT('Ctrl Pts',(-17.6596205619409,-3.49018656101197,177.97443488127));
#1586=CARTESIAN_POINT('Ctrl Pts',(-17.7200302505161,-3.18263533348267,177.52578108399));
#1587=CARTESIAN_POINT('Ctrl Pts',(-17.8327425616729,-2.47424944224197,176.81739519275));
#1588=CARTESIAN_POINT('Ctrl Pts',(-17.8924945311419,-2.02558278587652,176.509820096788));
#1589=CARTESIAN_POINT('Ctrl Pts',(-17.9766962279685,-1.04054739507664,176.101076729386));
#1590=CARTESIAN_POINT('Ctrl Pts',(-18.,-0.504043057803209,176.));
#1591=CARTESIAN_POINT('Ctrl Pts',(-18.,9.71445146547012E-16,176.));
#1592=CARTESIAN_POINT('',(-18.,-2.28179408289685E-15,184.));
#1593=CARTESIAN_POINT('Ctrl Pts',(-18.,-2.77555756156289E-15,176.));
#1594=CARTESIAN_POINT('Ctrl Pts',(-18.,0.504043057803207,176.));
#1595=CARTESIAN_POINT('Ctrl Pts',(-17.9766962279685,1.04054739507664,176.101076729386));
#1596=CARTESIAN_POINT('Ctrl Pts',(-17.8924945311419,2.02558278587652,176.509820096788));
#1597=CARTESIAN_POINT('Ctrl Pts',(-17.8327425616729,2.47424944224197,176.81739519275));
#1598=CARTESIAN_POINT('Ctrl Pts',(-17.7200302505161,3.18263533348267,177.52578108399));
#1599=CARTESIAN_POINT('Ctrl Pts',(-17.6596205619409,3.49018656101197,177.97443488127));
#1600=CARTESIAN_POINT('Ctrl Pts',(-17.5739034455062,3.89891257329756,178.959425202916));
#1601=CARTESIAN_POINT('Ctrl Pts',(-17.5499287747842,3.99999999999999,179.495913499213));
#1602=CARTESIAN_POINT('Ctrl Pts',(-17.5499287747842,3.99999999999999,180.));
#1603=CARTESIAN_POINT('Ctrl Pts',(-17.5499287747842,3.99999999999999,180.504086500787));
#1604=CARTESIAN_POINT('Ctrl Pts',(-17.5739034455062,3.89891257329756,181.040574797084));
#1605=CARTESIAN_POINT('Ctrl Pts',(-17.6596205619409,3.49018656101197,182.02556511873));
#1606=CARTESIAN_POINT('Ctrl Pts',(-17.7200302505161,3.18263533348267,182.47421891601));
#1607=CARTESIAN_POINT('Ctrl Pts',(-17.8327425616729,2.47424944224197,183.18260480725));
#1608=CARTESIAN_POINT('Ctrl Pts',(-17.8924945311419,2.02558278587652,183.490179903212));
#1609=CARTESIAN_POINT('Ctrl Pts',(-17.9766962279685,1.04054739507664,183.898923270614));
#1610=CARTESIAN_POINT('Ctrl Pts',(-18.,0.50404305780321,184.));
#1611=CARTESIAN_POINT('Ctrl Pts',(-18.,6.93889390390723E-16,184.));
#1612=CARTESIAN_POINT('Ctrl Pts',(-18.,7.63278329429795E-16,184.));
#1613=CARTESIAN_POINT('Ctrl Pts',(-18.,-0.504043057803209,184.));
#1614=CARTESIAN_POINT('Ctrl Pts',(-17.9766962279685,-1.04054739507664,183.898923270614));
#1615=CARTESIAN_POINT('Ctrl Pts',(-17.8924945311419,-2.02558278587652,183.490179903212));
#1616=CARTESIAN_POINT('Ctrl Pts',(-17.8327425616729,-2.47424944224197,183.18260480725));
#1617=CARTESIAN_POINT('Ctrl Pts',(-17.7200302505161,-3.18263533348267,182.47421891601));
#1618=CARTESIAN_POINT('Ctrl Pts',(-17.6596205619409,-3.49018656101197,182.02556511873));
#1619=CARTESIAN_POINT('Ctrl Pts',(-17.5739034455062,-3.89891257329756,181.040574797084));
#1620=CARTESIAN_POINT('Ctrl Pts',(-17.5499287747842,-3.99999999999999,180.504086500787));
#1621=CARTESIAN_POINT('Ctrl Pts',(-17.5499287747842,-3.99999999999999,180.));
#1622=CARTESIAN_POINT('Ctrl Pts',(-19.5959179422654,-3.99999999999999,180.));
#1623=CARTESIAN_POINT('Ctrl Pts',(-19.5959179422654,-3.99999999999999,180.503727007854));
#1624=CARTESIAN_POINT('Ctrl Pts',(-19.6173550647379,-3.89905118499443,181.040071108648));
#1625=CARTESIAN_POINT('Ctrl Pts',(-19.6941660317108,-3.4904216705935,182.02516802012));
#1626=CARTESIAN_POINT('Ctrl Pts',(-19.7483634040773,-3.18281240876835,182.474041840724));
#1627=CARTESIAN_POINT('Ctrl Pts',(-19.8496135055327,-2.47406169858037,183.182792550912));
#1628=CARTESIAN_POINT('Ctrl Pts',(-19.9033338860745,-2.02517944479051,183.490417366179));
#1629=CARTESIAN_POINT('Ctrl Pts',(-19.9790475458833,-1.04005322432747,183.899058168943));
#1630=CARTESIAN_POINT('Ctrl Pts',(-20.,-0.503698781685596,184.));
#1631=CARTESIAN_POINT('Ctrl Pts',(-20.,3.46944695195361E-16,184.));
#1632=CARTESIAN_POINT('Origin',(0.,0.,180.));
#1633=CARTESIAN_POINT('',(17.5499287747842,3.99999999999999,180.));
#1634=CARTESIAN_POINT('',(17.5499287747842,-3.99999999999999,180.));
#1635=CARTESIAN_POINT('Ctrl Pts',(17.5499287747842,3.99999999999999,180.));
#1636=CARTESIAN_POINT('Ctrl Pts',(17.5499287747842,3.99999999999999,180.504086500787));
#1637=CARTESIAN_POINT('Ctrl Pts',(17.5739034455062,3.89891257329756,181.040574797084));
#1638=CARTESIAN_POINT('Ctrl Pts',(17.6596205619409,3.49018656101197,182.02556511873));
#1639=CARTESIAN_POINT('Ctrl Pts',(17.7200302505161,3.18263533348267,182.47421891601));
#1640=CARTESIAN_POINT('Ctrl Pts',(17.8327425616729,2.47424944224197,183.18260480725));
#1641=CARTESIAN_POINT('Ctrl Pts',(17.8924945311419,2.0255827858765,183.490179903212));
#1642=CARTESIAN_POINT('Ctrl Pts',(17.9766962279685,1.04054739507661,183.898923270614));
#1643=CARTESIAN_POINT('Ctrl Pts',(18.,0.50404305780321,184.));
#1644=CARTESIAN_POINT('Ctrl Pts',(18.,-0.504043057803209,184.));
#1645=CARTESIAN_POINT('Ctrl Pts',(17.9766962279685,-1.04054739507664,183.898923270614));
#1646=CARTESIAN_POINT('Ctrl Pts',(17.8924945311419,-2.02558278587652,183.490179903212));
#1647=CARTESIAN_POINT('Ctrl Pts',(17.8327425616729,-2.47424944224197,183.18260480725));
#1648=CARTESIAN_POINT('Ctrl Pts',(17.7200302505161,-3.18263533348267,182.47421891601));
#1649=CARTESIAN_POINT('Ctrl Pts',(17.6596205619409,-3.49018656101197,182.02556511873));
#1650=CARTESIAN_POINT('Ctrl Pts',(17.5739034455062,-3.89891257329756,181.040574797084));
#1651=CARTESIAN_POINT('Ctrl Pts',(17.5499287747842,-3.99999999999999,180.504086500787));
#1652=CARTESIAN_POINT('Ctrl Pts',(17.5499287747842,-3.99999999999999,180.));
#1653=CARTESIAN_POINT('Ctrl Pts',(17.5499287747842,-3.99999999999999,180.));
#1654=CARTESIAN_POINT('Ctrl Pts',(17.5499287747842,-3.99999999999999,179.495913499213));
#1655=CARTESIAN_POINT('Ctrl Pts',(17.5739034455062,-3.89891257329756,178.959425202916));
#1656=CARTESIAN_POINT('Ctrl Pts',(17.6596205619409,-3.49018656101197,177.97443488127));
#1657=CARTESIAN_POINT('Ctrl Pts',(17.7200302505161,-3.18263533348267,177.52578108399));
#1658=CARTESIAN_POINT('Ctrl Pts',(17.8327425616729,-2.47424944224197,176.81739519275));
#1659=CARTESIAN_POINT('Ctrl Pts',(17.8924945311419,-2.02558278587652,176.509820096788));
#1660=CARTESIAN_POINT('Ctrl Pts',(17.9766962279685,-1.04054739507664,176.101076729386));
#1661=CARTESIAN_POINT('Ctrl Pts',(18.,-0.50404305780321,176.));
#1662=CARTESIAN_POINT('Ctrl Pts',(18.,0.504043057803209,176.));
#1663=CARTESIAN_POINT('Ctrl Pts',(17.9766962279685,1.04054739507664,176.101076729386));
#1664=CARTESIAN_POINT('Ctrl Pts',(17.8924945311419,2.02558278587652,176.509820096788));
#1665=CARTESIAN_POINT('Ctrl Pts',(17.8327425616729,2.47424944224197,176.81739519275));
#1666=CARTESIAN_POINT('Ctrl Pts',(17.7200302505161,3.18263533348267,177.52578108399));
#1667=CARTESIAN_POINT('Ctrl Pts',(17.6596205619409,3.49018656101197,177.97443488127));
#1668=CARTESIAN_POINT('Ctrl Pts',(17.5739034455062,3.89891257329756,178.959425202916));
#1669=CARTESIAN_POINT('Ctrl Pts',(17.5499287747842,3.99999999999999,179.495913499213));
#1670=CARTESIAN_POINT('Ctrl Pts',(17.5499287747842,3.99999999999999,180.));
#1671=CARTESIAN_POINT('',(19.5959179422654,-3.99999999999999,180.));
#1672=CARTESIAN_POINT('',(0.,-3.99999999999999,180.));
#1673=CARTESIAN_POINT('',(19.5959179422654,3.99999999999999,180.));
#1674=CARTESIAN_POINT('Ctrl Pts',(19.5959179422654,3.99999999999999,180.));
#1675=CARTESIAN_POINT('Ctrl Pts',(19.5959179422654,3.99999999999999,179.496272992146));
#1676=CARTESIAN_POINT('Ctrl Pts',(19.6173550647379,3.89905118499443,178.959928891352));
#1677=CARTESIAN_POINT('Ctrl Pts',(19.6941660317108,3.4904216705935,177.97483197988));
#1678=CARTESIAN_POINT('Ctrl Pts',(19.7483634040773,3.18281240876835,177.525958159276));
#1679=CARTESIAN_POINT('Ctrl Pts',(19.8496135055327,2.47406169858037,176.817207449088));
#1680=CARTESIAN_POINT('Ctrl Pts',(19.9033338860745,2.02517944479051,176.509582633821));
#1681=CARTESIAN_POINT('Ctrl Pts',(19.9790475458833,1.04005322432747,176.100941831057));
#1682=CARTESIAN_POINT('Ctrl Pts',(20.,0.503698781685596,176.));
#1683=CARTESIAN_POINT('Ctrl Pts',(20.,-0.503698781685597,176.));
#1684=CARTESIAN_POINT('Ctrl Pts',(19.9790475458833,-1.04005322432747,176.100941831057));
#1685=CARTESIAN_POINT('Ctrl Pts',(19.9033338860745,-2.02517944479051,176.509582633821));
#1686=CARTESIAN_POINT('Ctrl Pts',(19.8496135055327,-2.47406169858037,176.817207449088));
#1687=CARTESIAN_POINT('Ctrl Pts',(19.7483634040773,-3.18281240876835,177.525958159276));
#1688=CARTESIAN_POINT('Ctrl Pts',(19.6941660317108,-3.4904216705935,177.97483197988));
#1689=CARTESIAN_POINT('Ctrl Pts',(19.6173550647379,-3.89905118499443,178.959928891352));
#1690=CARTESIAN_POINT('Ctrl Pts',(19.5959179422654,-3.99999999999999,179.496272992146));
#1691=CARTESIAN_POINT('Ctrl Pts',(19.5959179422654,-3.99999999999999,180.));
#1692=CARTESIAN_POINT('Ctrl Pts',(19.5959179422654,-3.99999999999999,180.));
#1693=CARTESIAN_POINT('Ctrl Pts',(19.5959179422654,-3.99999999999999,180.503727007854));
#1694=CARTESIAN_POINT('Ctrl Pts',(19.6173550647379,-3.89905118499443,181.040071108648));
#1695=CARTESIAN_POINT('Ctrl Pts',(19.6941660317108,-3.49042167059349,182.02516802012));
#1696=CARTESIAN_POINT('Ctrl Pts',(19.7483634040773,-3.18281240876835,182.474041840724));
#1697=CARTESIAN_POINT('Ctrl Pts',(19.8496135055327,-2.47406169858037,183.182792550912));
#1698=CARTESIAN_POINT('Ctrl Pts',(19.9033338860745,-2.02517944479048,183.490417366179));
#1699=CARTESIAN_POINT('Ctrl Pts',(19.9790475458833,-1.04005322432745,183.899058168943));
#1700=CARTESIAN_POINT('Ctrl Pts',(20.,-0.503698781685597,184.));
#1701=CARTESIAN_POINT('Ctrl Pts',(20.,0.503698781685597,184.));
#1702=CARTESIAN_POINT('Ctrl Pts',(19.9790475458833,1.04005322432747,183.899058168943));
#1703=CARTESIAN_POINT('Ctrl Pts',(19.9033338860745,2.02517944479051,183.490417366179));
#1704=CARTESIAN_POINT('Ctrl Pts',(19.8496135055327,2.47406169858037,183.182792550912));
#1705=CARTESIAN_POINT('Ctrl Pts',(19.7483634040773,3.18281240876835,182.474041840724));
#1706=CARTESIAN_POINT('Ctrl Pts',(19.6941660317108,3.4904216705935,182.02516802012));
#1707=CARTESIAN_POINT('Ctrl Pts',(19.6173550647379,3.89905118499443,181.040071108648));
#1708=CARTESIAN_POINT('Ctrl Pts',(19.5959179422654,3.99999999999999,180.503727007854));
#1709=CARTESIAN_POINT('Ctrl Pts',(19.5959179422654,3.99999999999999,180.));
#1710=CARTESIAN_POINT('Origin',(0.,0.,0.));
#1711=CARTESIAN_POINT('',(-18.,2.20436423846524E-15,2.));
#1712=CARTESIAN_POINT('Origin',(0.,0.,2.));
#1713=CARTESIAN_POINT('',(-18.,-2.20436423846524E-15,0.));
#1714=CARTESIAN_POINT('',(-18.,-2.20436423846524E-15,200.));
#1715=CARTESIAN_POINT('',(-18.,-2.20436423846524E-15,0.));
#1716=CARTESIAN_POINT('Origin',(0.,0.,200.));
#1717=CARTESIAN_POINT('Origin',(0.,0.,0.));
#1718=CARTESIAN_POINT('',(-20.,-2.44929359829471E-15,200.));
#1719=CARTESIAN_POINT('Origin',(0.,0.,200.));
#1720=CARTESIAN_POINT('',(-20.,-2.44929359829471E-15,0.));
#1721=CARTESIAN_POINT('',(-20.,-2.44929359829471E-15,2.));
#1722=CARTESIAN_POINT('',(-20.,-2.44929359829471E-15,0.));
#1723=CARTESIAN_POINT('Origin',(0.,0.,2.));
#1724=CARTESIAN_POINT('Origin',(0.,0.,200.));
#1725=CARTESIAN_POINT('Origin',(0.,0.,2.));
#1726=CARTESIAN_POINT('',(0.,0.,0.));
#1727=CARTESIAN_POINT('Origin',(0.,0.,1.));
#1728=CARTESIAN_POINT('',(-20.,2.44929359829471E-15,1.));
#1729=CARTESIAN_POINT('Origin',(0.,0.,1.));
#1730=CARTESIAN_POINT('Origin',(0.,0.,0.));
#1731=CARTESIAN_POINT('',(-20.,2.44929359829471E-15,8.));
#1732=CARTESIAN_POINT('',(-20.,-2.44929359829471E-15,0.));
#1733=CARTESIAN_POINT('Origin',(0.,0.,8.));
#1734=CARTESIAN_POINT('Origin',(0.,0.,0.));
#1735=CARTESIAN_POINT('',(-24.,2.93915231795365E-15,8.));
#1736=CARTESIAN_POINT('Origin',(0.,0.,8.));
#1737=CARTESIAN_POINT('',(-24.,2.93915231795365E-15,0.));
#1738=CARTESIAN_POINT('',(-24.,-2.93915231795365E-15,0.));
#1739=CARTESIAN_POINT('Origin',(0.,0.,0.));
#1740=CARTESIAN_POINT('Origin',(0.,0.,0.));
#1741=CARTESIAN_POINT('Origin',(0.,0.,8.));
#1742=CARTESIAN_POINT('',(0.,0.,0.));
#1743=CARTESIAN_POINT('Origin',(-17.,0.,316.));
#1744=CARTESIAN_POINT('',(-17.,-9.,324.));
#1745=CARTESIAN_POINT('',(-17.,9.,324.));
#1746=CARTESIAN_POINT('',(-17.,0.,324.));
#1747=CARTESIAN_POINT('',(-17.,9.,316.));
#1748=CARTESIAN_POINT('',(-17.,9.,324.));
#1749=CARTESIAN_POINT('',(-17.,-9.,316.));
#1750=CARTESIAN_POINT('',(-17.,0.,316.));
#1751=CARTESIAN_POINT('',(-17.,-9.,324.));
#1752=CARTESIAN_POINT('Origin',(-17.,0.,324.));
#1753=CARTESIAN_POINT('',(-15.,-9.,324.));
#1754=CARTESIAN_POINT('',(-15.,9.,324.));
#1755=CARTESIAN_POINT('',(-15.,0.,324.));
#1756=CARTESIAN_POINT('',(-17.,9.,324.));
#1757=CARTESIAN_POINT('',(-17.,-9.,324.));
#1758=CARTESIAN_POINT('Origin',(-15.,0.,324.));
#1759=CARTESIAN_POINT('',(-15.,-9.,316.));
#1760=CARTESIAN_POINT('',(-15.,9.,316.));
#1761=CARTESIAN_POINT('',(-15.,0.,316.));
#1762=CARTESIAN_POINT('',(-15.,9.,324.));
#1763=CARTESIAN_POINT('',(-15.,-9.,324.));
#1764=CARTESIAN_POINT('Ctrl Pts',(-15.,-9.01917151683795,316.));
#1765=CARTESIAN_POINT('Ctrl Pts',(-15.,12.6038343033676,316.));
#1766=CARTESIAN_POINT('Ctrl Pts',(-15.,-9.01917151683795,312.917218954967));
#1767=CARTESIAN_POINT('Ctrl Pts',(-15.,12.6038343033676,312.917218954967));
#1768=CARTESIAN_POINT('Ctrl Pts',(-14.9804665025967,-9.01917151683795,309.284971969759));
#1769=CARTESIAN_POINT('Ctrl Pts',(-14.9804665025967,12.6038343033676,309.284971969759));
#1770=CARTESIAN_POINT('Ctrl Pts',(-14.8743203079702,-9.01917151683795,305.389849883143));
#1771=CARTESIAN_POINT('Ctrl Pts',(-14.8743203079702,12.6038343033676,305.389849883143));
#1772=CARTESIAN_POINT('Ctrl Pts',(-14.7151010160305,-9.01917151683795,299.547166753218));
#1773=CARTESIAN_POINT('Ctrl Pts',(-14.7151010160305,12.6038343033676,299.547166753218));
#1774=CARTESIAN_POINT('Ctrl Pts',(-14.3613339472215,-9.01917151683795,293.114195242939));
#1775=CARTESIAN_POINT('Ctrl Pts',(-14.3613339472215,12.6038343033676,293.114195242939));
#1776=CARTESIAN_POINT('Ctrl Pts',(-12.5329121501934,-9.01917151683795,288.887907445925));
#1777=CARTESIAN_POINT('Ctrl Pts',(-12.5329121501934,12.6038343033676,288.887907445925));
#1778=CARTESIAN_POINT('Ctrl Pts',(-11.3428854490917,-9.01917151683795,286.13723179047));
#1779=CARTESIAN_POINT('Ctrl Pts',(-11.3428854490917,12.6038343033676,286.13723179047));
#1780=CARTESIAN_POINT('Ctrl Pts',(-9.6259837213127,-9.01917151683795,284.320800585332));
#1781=CARTESIAN_POINT('Ctrl Pts',(-9.6259837213127,12.6038343033676,284.320800585332));
#1782=CARTESIAN_POINT('Ctrl Pts',(-6.96718239188881,-9.01917151683795,283.179505866003));
#1783=CARTESIAN_POINT('Ctrl Pts',(-6.96718239188881,12.6038343033676,283.179505866003));
#1784=CARTESIAN_POINT('Ctrl Pts',(-5.58089918248474,-9.01917151683795,282.584441583133));
#1785=CARTESIAN_POINT('Ctrl Pts',(-5.58089918248474,12.6038343033676,282.584441583133));
#1786=CARTESIAN_POINT('Ctrl Pts',(-3.9277760249776,-9.01917151683795,282.184209001161));
#1787=CARTESIAN_POINT('Ctrl Pts',(-3.9277760249776,12.6038343033676,282.184209001161));
#1788=CARTESIAN_POINT('Ctrl Pts',(-2.00000000000228,-9.01917151683795,282.007690234858));
#1789=CARTESIAN_POINT('Ctrl Pts',(-2.00000000000228,12.6038343033676,282.007690234858));
#1790=CARTESIAN_POINT('Ctrl Pts',(-1.94431052069769,-9.01917151683795,282.002590971222));
#1791=CARTESIAN_POINT('Ctrl Pts',(-1.94431052069769,12.6038343033676,282.002590971222));
#1792=CARTESIAN_POINT('Ctrl Pts',(-1.88839473154277,-9.01917151683795,281.997678278411));
#1793=CARTESIAN_POINT('Ctrl Pts',(-1.88839473154277,12.6038343033676,281.997678278411));
#1794=CARTESIAN_POINT('Ctrl Pts',(-1.8322528584517,-9.01917151683795,281.992952808398));
#1795=CARTESIAN_POINT('Ctrl Pts',(-1.8322528584517,12.6038343033676,281.992952808398));
#1796=CARTESIAN_POINT('Ctrl Pts',(-0.067982678772372,-9.01917151683795,
281.844453918553));
#1797=CARTESIAN_POINT('Ctrl Pts',(-0.067982678772372,12.6038343033676,281.844453918553));
#1798=CARTESIAN_POINT('Ctrl Pts',(1.69628750090713,-9.01917151683795,281.695955028709));
#1799=CARTESIAN_POINT('Ctrl Pts',(1.69628750090713,12.6038343033676,281.695955028709));
#1800=CARTESIAN_POINT('Ctrl Pts',(3.46055768058644,-9.01917151683795,281.547456138864));
#1801=CARTESIAN_POINT('Ctrl Pts',(3.46055768058644,12.6038343033676,281.547456138864));
#1802=CARTESIAN_POINT('',(-2.61075883134509E-14,-9.,281.838731806123));
#1803=CARTESIAN_POINT('',(-2.61075883134509E-14,9.,281.838731806123));
#1804=CARTESIAN_POINT('',(-5.91540705308091E-14,9.,281.838731806123));
#1805=CARTESIAN_POINT('Ctrl Pts',(-15.,9.,316.));
#1806=CARTESIAN_POINT('Ctrl Pts',(-15.,9.,312.917218954967));
#1807=CARTESIAN_POINT('Ctrl Pts',(-14.9804665025967,9.,309.284971969759));
#1808=CARTESIAN_POINT('Ctrl Pts',(-14.8743203079702,9.,305.389849883143));
#1809=CARTESIAN_POINT('Ctrl Pts',(-14.7151010160305,9.,299.547166753218));
#1810=CARTESIAN_POINT('Ctrl Pts',(-14.3613339472215,9.,293.114195242939));
#1811=CARTESIAN_POINT('Ctrl Pts',(-12.5329121501934,9.,288.887907445925));
#1812=CARTESIAN_POINT('Ctrl Pts',(-11.3428854490917,9.,286.13723179047));
#1813=CARTESIAN_POINT('Ctrl Pts',(-9.6259837213127,9.,284.320800585332));
#1814=CARTESIAN_POINT('Ctrl Pts',(-6.96718239188881,9.,283.179505866003));
#1815=CARTESIAN_POINT('Ctrl Pts',(-5.58089918248474,9.,282.584441583133));
#1816=CARTESIAN_POINT('Ctrl Pts',(-3.9277760249776,9.,282.184209001161));
#1817=CARTESIAN_POINT('Ctrl Pts',(-2.00000000000228,9.,282.007690234858));
#1818=CARTESIAN_POINT('Ctrl Pts',(-1.94431052069769,9.,282.002590971222));
#1819=CARTESIAN_POINT('Ctrl Pts',(-1.88839473154277,9.,281.997678278411));
#1820=CARTESIAN_POINT('Ctrl Pts',(-1.8322528584517,9.,281.992952808398));
#1821=CARTESIAN_POINT('Ctrl Pts',(-1.22150190563454,9.,281.941545807639));
#1822=CARTESIAN_POINT('Ctrl Pts',(-0.610750952817352,9.,281.890138806881));
#1823=CARTESIAN_POINT('Ctrl Pts',(-1.61426427780498E-13,9.,281.838731806122));
#1824=CARTESIAN_POINT('Ctrl Pts',(-1.39499523044151E-13,-9.,281.838731806122));
#1825=CARTESIAN_POINT('Ctrl Pts',(-0.610750952817337,-9.,281.890138806881));
#1826=CARTESIAN_POINT('Ctrl Pts',(-1.22150190563453,-9.,281.941545807639));
#1827=CARTESIAN_POINT('Ctrl Pts',(-1.8322528584517,-9.,281.992952808398));
#1828=CARTESIAN_POINT('Ctrl Pts',(-1.88839473154277,-9.,281.997678278411));
#1829=CARTESIAN_POINT('Ctrl Pts',(-1.94431052069769,-9.,282.002590971222));
#1830=CARTESIAN_POINT('Ctrl Pts',(-2.00000000000228,-9.,282.007690234858));
#1831=CARTESIAN_POINT('Ctrl Pts',(-3.9277760249776,-9.,282.184209001161));
#1832=CARTESIAN_POINT('Ctrl Pts',(-5.58089918248474,-9.,282.584441583133));
#1833=CARTESIAN_POINT('Ctrl Pts',(-6.96718239188881,-9.,283.179505866003));
#1834=CARTESIAN_POINT('Ctrl Pts',(-9.6259837213127,-9.,284.320800585332));
#1835=CARTESIAN_POINT('Ctrl Pts',(-11.3428854490917,-9.,286.13723179047));
#1836=CARTESIAN_POINT('Ctrl Pts',(-12.5329121501934,-9.,288.887907445925));
#1837=CARTESIAN_POINT('Ctrl Pts',(-14.3613339472215,-9.,293.114195242939));
#1838=CARTESIAN_POINT('Ctrl Pts',(-14.7151010160305,-9.,299.547166753218));
#1839=CARTESIAN_POINT('Ctrl Pts',(-14.8743203079702,-9.,305.389849883143));
#1840=CARTESIAN_POINT('Ctrl Pts',(-14.9804665025967,-9.,309.284971969759));
#1841=CARTESIAN_POINT('Ctrl Pts',(-15.,-9.,312.917218954967));
#1842=CARTESIAN_POINT('Ctrl Pts',(-15.,-9.,316.));
#1843=CARTESIAN_POINT('Ctrl Pts',(3.,-9.,279.579149238152));
#1844=CARTESIAN_POINT('Ctrl Pts',(3.,12.6,279.579149238152));
#1845=CARTESIAN_POINT('Ctrl Pts',(2.,-9.,279.663319390522));
#1846=CARTESIAN_POINT('Ctrl Pts',(2.,12.6,279.663319390522));
#1847=CARTESIAN_POINT('Ctrl Pts',(1.,-9.,279.747489542891));
#1848=CARTESIAN_POINT('Ctrl Pts',(1.,12.6,279.747489542891));
#1849=CARTESIAN_POINT('Ctrl Pts',(-5.55111512312578E-16,-9.,279.831659695261));
#1850=CARTESIAN_POINT('Ctrl Pts',(-5.55111512312578E-16,12.6,279.831659695261));
#1851=CARTESIAN_POINT('Ctrl Pts',(-1.,-9.,279.91582984763));
#1852=CARTESIAN_POINT('Ctrl Pts',(-1.,12.6,279.91582984763));
#1853=CARTESIAN_POINT('Ctrl Pts',(-2.,-9.,280.));
#1854=CARTESIAN_POINT('Ctrl Pts',(-2.,12.6,280.));
#1855=CARTESIAN_POINT('Ctrl Pts',(-2.66368424066569,-9.,280.055862403662));
#1856=CARTESIAN_POINT('Ctrl Pts',(-2.66368424066569,12.6,280.055862403662));
#1857=CARTESIAN_POINT('Ctrl Pts',(-3.9517913938126,-9.,280.208504145521));
#1858=CARTESIAN_POINT('Ctrl Pts',(-3.9517913938126,12.6,280.208504145521));
#1859=CARTESIAN_POINT('Ctrl Pts',(-5.76616670029465,-9.,280.560219196132));
#1860=CARTESIAN_POINT('Ctrl Pts',(-5.76616670029465,12.6,280.560219196132));
#1861=CARTESIAN_POINT('Ctrl Pts',(-7.94806288019228,-9.,281.276448102944));
#1862=CARTESIAN_POINT('Ctrl Pts',(-7.94806288019228,12.6,281.276448102944));
#1863=CARTESIAN_POINT('Ctrl Pts',(-10.2723403348262,-9.,282.590975648728));
#1864=CARTESIAN_POINT('Ctrl Pts',(-10.2723403348262,12.6,282.590975648728));
#1865=CARTESIAN_POINT('Ctrl Pts',(-12.1890242800701,-9.,284.326851421562));
#1866=CARTESIAN_POINT('Ctrl Pts',(-12.1890242800701,12.6,284.326851421562));
#1867=CARTESIAN_POINT('Ctrl Pts',(-13.7033484644208,-9.,286.473438815185));
#1868=CARTESIAN_POINT('Ctrl Pts',(-13.7033484644208,12.6,286.473438815185));
#1869=CARTESIAN_POINT('Ctrl Pts',(-14.8403951587419,-9.,288.995763819941));
#1870=CARTESIAN_POINT('Ctrl Pts',(-14.8403951587419,12.6,288.995763819941));
#1871=CARTESIAN_POINT('Ctrl Pts',(-15.6496061172615,-9.,291.82914277586));
#1872=CARTESIAN_POINT('Ctrl Pts',(-15.6496061172615,12.6,291.82914277586));
#1873=CARTESIAN_POINT('Ctrl Pts',(-16.1926929497518,-9.,294.892205598351));
#1874=CARTESIAN_POINT('Ctrl Pts',(-16.1926929497518,12.6,294.892205598351));
#1875=CARTESIAN_POINT('Ctrl Pts',(-16.5359735439045,-9.,298.095070696299));
#1876=CARTESIAN_POINT('Ctrl Pts',(-16.5359735439045,12.6,298.095070696299));
#1877=CARTESIAN_POINT('Ctrl Pts',(-16.7422790149997,-9.,301.348120547886));
#1878=CARTESIAN_POINT('Ctrl Pts',(-16.7422790149997,12.6,301.348120547886));
#1879=CARTESIAN_POINT('Ctrl Pts',(-16.8634487703245,-9.,304.57015716772));
#1880=CARTESIAN_POINT('Ctrl Pts',(-16.8634487703245,12.6,304.57015716772));
#1881=CARTESIAN_POINT('Ctrl Pts',(-16.9338349467122,-9.,307.69587590639));
#1882=CARTESIAN_POINT('Ctrl Pts',(-16.9338349467122,12.6,307.69587590639));
#1883=CARTESIAN_POINT('Ctrl Pts',(-16.9745170477256,-9.,310.674187150777));
#1884=CARTESIAN_POINT('Ctrl Pts',(-16.9745170477256,12.6,310.674187150777));
#1885=CARTESIAN_POINT('Ctrl Pts',(-16.9920318646118,-9.,312.909176752281));
#1886=CARTESIAN_POINT('Ctrl Pts',(-16.9920318646118,12.6,312.909176752281));
#1887=CARTESIAN_POINT('Ctrl Pts',(-16.9985513080952,-9.,314.491917916066));
#1888=CARTESIAN_POINT('Ctrl Pts',(-16.9985513080952,12.6,314.491917916066));
#1889=CARTESIAN_POINT('Ctrl Pts',(-17.,-9.,315.50441646936));
#1890=CARTESIAN_POINT('Ctrl Pts',(-17.,12.6,315.50441646936));
#1891=CARTESIAN_POINT('Ctrl Pts',(-17.,-9.,316.));
#1892=CARTESIAN_POINT('Ctrl Pts',(-17.,12.6,316.));
#1893=CARTESIAN_POINT('',(-1.13335267097151E-15,9.,279.831659695261));
#1894=CARTESIAN_POINT('Ctrl Pts',(-17.,9.,316.));
#1895=CARTESIAN_POINT('Ctrl Pts',(-17.,9.,315.50441646936));
#1896=CARTESIAN_POINT('Ctrl Pts',(-16.9985513080952,9.,314.491917916066));
#1897=CARTESIAN_POINT('Ctrl Pts',(-16.9920318646118,9.,312.909176752281));
#1898=CARTESIAN_POINT('Ctrl Pts',(-16.9745170477256,9.,310.674187150777));
#1899=CARTESIAN_POINT('Ctrl Pts',(-16.9338349467122,9.,307.69587590639));
#1900=CARTESIAN_POINT('Ctrl Pts',(-16.8634487703245,9.,304.57015716772));
#1901=CARTESIAN_POINT('Ctrl Pts',(-16.7422790149997,9.,301.348120547886));
#1902=CARTESIAN_POINT('Ctrl Pts',(-16.5359735439045,9.,298.095070696299));
#1903=CARTESIAN_POINT('Ctrl Pts',(-16.1926929497518,9.,294.892205598351));
#1904=CARTESIAN_POINT('Ctrl Pts',(-15.6496061172615,9.,291.82914277586));
#1905=CARTESIAN_POINT('Ctrl Pts',(-14.8403951587419,9.,288.995763819941));
#1906=CARTESIAN_POINT('Ctrl Pts',(-13.7033484644208,9.,286.473438815185));
#1907=CARTESIAN_POINT('Ctrl Pts',(-12.1890242800701,9.,284.326851421562));
#1908=CARTESIAN_POINT('Ctrl Pts',(-10.2723403348262,9.,282.590975648728));
#1909=CARTESIAN_POINT('Ctrl Pts',(-7.94806288019228,9.,281.276448102944));
#1910=CARTESIAN_POINT('Ctrl Pts',(-5.76616670029465,9.,280.560219196132));
#1911=CARTESIAN_POINT('Ctrl Pts',(-3.9517913938126,9.,280.208504145521));
#1912=CARTESIAN_POINT('Ctrl Pts',(-2.66368424066569,9.,280.055862403662));
#1913=CARTESIAN_POINT('Ctrl Pts',(-1.60000000000001,9.,279.966331939052));
#1914=CARTESIAN_POINT('Ctrl Pts',(-1.20000000000001,9.,279.932663878104));
#1915=CARTESIAN_POINT('Ctrl Pts',(-0.800000000000013,9.,279.898995817156));
#1916=CARTESIAN_POINT('Ctrl Pts',(-0.400000000000013,9.,279.865327756209));
#1917=CARTESIAN_POINT('Ctrl Pts',(-2.04350425470068E-14,9.,279.831659695261));
#1918=CARTESIAN_POINT('',(-1.04083408558608E-15,-9.,279.831659695261));
#1919=CARTESIAN_POINT('',(-3.40005801291454E-15,9.,279.831659695261));
#1920=CARTESIAN_POINT('Ctrl Pts',(-17.,-9.,316.));
#1921=CARTESIAN_POINT('Ctrl Pts',(-17.,-9.,315.50441646936));
#1922=CARTESIAN_POINT('Ctrl Pts',(-16.9985513080952,-9.,314.491917916066));
#1923=CARTESIAN_POINT('Ctrl Pts',(-16.9920318646118,-9.,312.909176752281));
#1924=CARTESIAN_POINT('Ctrl Pts',(-16.9745170477256,-9.,310.674187150777));
#1925=CARTESIAN_POINT('Ctrl Pts',(-16.9338349467122,-9.,307.69587590639));
#1926=CARTESIAN_POINT('Ctrl Pts',(-16.8634487703245,-9.,304.57015716772));
#1927=CARTESIAN_POINT('Ctrl Pts',(-16.7422790149997,-9.,301.348120547886));
#1928=CARTESIAN_POINT('Ctrl Pts',(-16.5359735439045,-9.,298.095070696299));
#1929=CARTESIAN_POINT('Ctrl Pts',(-16.1926929497518,-9.,294.892205598351));
#1930=CARTESIAN_POINT('Ctrl Pts',(-15.6496061172615,-9.,291.82914277586));
#1931=CARTESIAN_POINT('Ctrl Pts',(-14.8403951587419,-9.,288.995763819941));
#1932=CARTESIAN_POINT('Ctrl Pts',(-13.7033484644208,-9.,286.473438815185));
#1933=CARTESIAN_POINT('Ctrl Pts',(-12.1890242800701,-9.,284.326851421562));
#1934=CARTESIAN_POINT('Ctrl Pts',(-10.2723403348262,-9.,282.590975648728));
#1935=CARTESIAN_POINT('Ctrl Pts',(-7.94806288019228,-9.,281.276448102944));
#1936=CARTESIAN_POINT('Ctrl Pts',(-5.76616670029465,-9.,280.560219196132));
#1937=CARTESIAN_POINT('Ctrl Pts',(-3.9517913938126,-9.,280.208504145521));
#1938=CARTESIAN_POINT('Ctrl Pts',(-2.66368424066569,-9.,280.055862403662));
#1939=CARTESIAN_POINT('Ctrl Pts',(-1.60000000000001,-9.,279.966331939052));
#1940=CARTESIAN_POINT('Ctrl Pts',(-1.20000000000001,-9.,279.932663878104));
#1941=CARTESIAN_POINT('Ctrl Pts',(-0.800000000000013,-9.,279.898995817156));
#1942=CARTESIAN_POINT('Ctrl Pts',(-0.400000000000013,-9.,279.865327756209));
#1943=CARTESIAN_POINT('Ctrl Pts',(-2.04350425470068E-14,-9.,279.831659695261));
#1944=CARTESIAN_POINT('Origin',(2.,9.,302.));
#1945=CARTESIAN_POINT('',(15.,9.,316.));
#1946=CARTESIAN_POINT('Ctrl Pts',(-8.59312621059871E-14,9.,281.838731806122));
#1947=CARTESIAN_POINT('Ctrl Pts',(0.610750952817164,9.,281.890138806881));
#1948=CARTESIAN_POINT('Ctrl Pts',(1.22150190563442,9.,281.941545807639));
#1949=CARTESIAN_POINT('Ctrl Pts',(1.8322528584517,9.,281.992952808398));
#1950=CARTESIAN_POINT('Ctrl Pts',(1.88839473154122,9.,281.99767827841));
#1951=CARTESIAN_POINT('Ctrl Pts',(1.94431052069477,9.,282.002590971222));
#1952=CARTESIAN_POINT('Ctrl Pts',(1.99999999999782,9.,282.007690234858));
#1953=CARTESIAN_POINT('Ctrl Pts',(3.92777602497513,9.,282.18420900116));
#1954=CARTESIAN_POINT('Ctrl Pts',(5.58089918248363,9.,282.584441583133));
#1955=CARTESIAN_POINT('Ctrl Pts',(6.96718239188881,9.,283.179505866003));
#1956=CARTESIAN_POINT('Ctrl Pts',(9.62598372131269,9.,284.320800585332));
#1957=CARTESIAN_POINT('Ctrl Pts',(11.3428854490917,9.,286.13723179047));
#1958=CARTESIAN_POINT('Ctrl Pts',(12.5329121501934,9.,288.887907445925));
#1959=CARTESIAN_POINT('Ctrl Pts',(14.3613339472215,9.,293.114195242939));
#1960=CARTESIAN_POINT('Ctrl Pts',(14.7151010160305,9.,299.547166753218));
#1961=CARTESIAN_POINT('Ctrl Pts',(14.8743203079702,9.,305.389849883143));
#1962=CARTESIAN_POINT('Ctrl Pts',(14.9804665025967,9.,309.284971969759));
#1963=CARTESIAN_POINT('Ctrl Pts',(15.,9.,312.917218954967));
#1964=CARTESIAN_POINT('Ctrl Pts',(15.,9.,316.));
#1965=CARTESIAN_POINT('',(15.,9.,324.));
#1966=CARTESIAN_POINT('',(15.,9.,324.));
#1967=CARTESIAN_POINT('',(17.,9.,324.));
#1968=CARTESIAN_POINT('',(-13.,9.,324.));
#1969=CARTESIAN_POINT('',(17.,9.,316.));
#1970=CARTESIAN_POINT('',(17.,9.,324.));
#1971=CARTESIAN_POINT('Ctrl Pts',(7.73686670285656E-15,9.,279.831659695261));
#1972=CARTESIAN_POINT('Ctrl Pts',(0.400000000000004,9.,279.865327756209));
#1973=CARTESIAN_POINT('Ctrl Pts',(0.800000000000005,9.,279.898995817156));
#1974=CARTESIAN_POINT('Ctrl Pts',(1.2,9.,279.932663878104));
#1975=CARTESIAN_POINT('Ctrl Pts',(1.6,9.,279.966331939052));
#1976=CARTESIAN_POINT('Ctrl Pts',(2.66368424066569,9.,280.055862403662));
#1977=CARTESIAN_POINT('Ctrl Pts',(3.9517913938126,9.,280.208504145521));
#1978=CARTESIAN_POINT('Ctrl Pts',(5.76616670029465,9.,280.560219196132));
#1979=CARTESIAN_POINT('Ctrl Pts',(7.94806288019228,9.,281.276448102944));
#1980=CARTESIAN_POINT('Ctrl Pts',(10.2723403348262,9.,282.590975648728));
#1981=CARTESIAN_POINT('Ctrl Pts',(12.1890242800701,9.,284.326851421562));
#1982=CARTESIAN_POINT('Ctrl Pts',(13.7033484644208,9.,286.473438815185));
#1983=CARTESIAN_POINT('Ctrl Pts',(14.8403951587419,9.,288.995763819941));
#1984=CARTESIAN_POINT('Ctrl Pts',(15.6496061172615,9.,291.82914277586));
#1985=CARTESIAN_POINT('Ctrl Pts',(16.1926929497518,9.,294.892205598351));
#1986=CARTESIAN_POINT('Ctrl Pts',(16.5359735439045,9.,298.095070696299));
#1987=CARTESIAN_POINT('Ctrl Pts',(16.7422790149997,9.,301.348120547886));
#1988=CARTESIAN_POINT('Ctrl Pts',(16.8634487703245,9.,304.57015716772));
#1989=CARTESIAN_POINT('Ctrl Pts',(16.9338349467122,9.,307.69587590639));
#1990=CARTESIAN_POINT('Ctrl Pts',(16.9745170477256,9.,310.674187150777));
#1991=CARTESIAN_POINT('Ctrl Pts',(16.9920318646118,9.,312.909176752281));
#1992=CARTESIAN_POINT('Ctrl Pts',(16.9985513080952,9.,314.491917916066));
#1993=CARTESIAN_POINT('Ctrl Pts',(17.,9.,315.50441646936));
#1994=CARTESIAN_POINT('Ctrl Pts',(17.,9.,316.));
#1995=CARTESIAN_POINT('Origin',(2.,-9.,302.));
#1996=CARTESIAN_POINT('',(17.,-9.,316.));
#1997=CARTESIAN_POINT('Ctrl Pts',(7.73686670285656E-15,-9.,279.831659695261));
#1998=CARTESIAN_POINT('Ctrl Pts',(0.400000000000004,-9.,279.865327756209));
#1999=CARTESIAN_POINT('Ctrl Pts',(0.800000000000005,-9.,279.898995817156));
#2000=CARTESIAN_POINT('Ctrl Pts',(1.2,-9.,279.932663878104));
#2001=CARTESIAN_POINT('Ctrl Pts',(1.6,-9.,279.966331939052));
#2002=CARTESIAN_POINT('Ctrl Pts',(2.66368424066569,-9.,280.055862403662));
#2003=CARTESIAN_POINT('Ctrl Pts',(3.9517913938126,-9.,280.208504145521));
#2004=CARTESIAN_POINT('Ctrl Pts',(5.76616670029465,-9.,280.560219196132));
#2005=CARTESIAN_POINT('Ctrl Pts',(7.94806288019228,-9.,281.276448102944));
#2006=CARTESIAN_POINT('Ctrl Pts',(10.2723403348262,-9.,282.590975648728));
#2007=CARTESIAN_POINT('Ctrl Pts',(12.1890242800701,-9.,284.326851421562));
#2008=CARTESIAN_POINT('Ctrl Pts',(13.7033484644208,-9.,286.473438815185));
#2009=CARTESIAN_POINT('Ctrl Pts',(14.8403951587419,-9.,288.995763819941));
#2010=CARTESIAN_POINT('Ctrl Pts',(15.6496061172615,-9.,291.82914277586));
#2011=CARTESIAN_POINT('Ctrl Pts',(16.1926929497518,-9.,294.892205598351));
#2012=CARTESIAN_POINT('Ctrl Pts',(16.5359735439045,-9.,298.095070696299));
#2013=CARTESIAN_POINT('Ctrl Pts',(16.7422790149997,-9.,301.348120547886));
#2014=CARTESIAN_POINT('Ctrl Pts',(16.8634487703245,-9.,304.57015716772));
#2015=CARTESIAN_POINT('Ctrl Pts',(16.9338349467122,-9.,307.69587590639));
#2016=CARTESIAN_POINT('Ctrl Pts',(16.9745170477256,-9.,310.674187150777));
#2017=CARTESIAN_POINT('Ctrl Pts',(16.9920318646118,-9.,312.909176752281));
#2018=CARTESIAN_POINT('Ctrl Pts',(16.9985513080952,-9.,314.491917916066));
#2019=CARTESIAN_POINT('Ctrl Pts',(17.,-9.,315.50441646936));
#2020=CARTESIAN_POINT('Ctrl Pts',(17.,-9.,316.));
#2021=CARTESIAN_POINT('',(17.,-9.,324.));
#2022=CARTESIAN_POINT('',(17.,-9.,324.));
#2023=CARTESIAN_POINT('',(15.,-9.,324.));
#2024=CARTESIAN_POINT('',(-13.,-9.,324.));
#2025=CARTESIAN_POINT('',(15.,-9.,316.));
#2026=CARTESIAN_POINT('',(15.,-9.,324.));
#2027=CARTESIAN_POINT('Ctrl Pts',(15.,-9.,316.));
#2028=CARTESIAN_POINT('Ctrl Pts',(15.,-9.,312.917218954967));
#2029=CARTESIAN_POINT('Ctrl Pts',(14.9804665025967,-9.,309.284971969759));
#2030=CARTESIAN_POINT('Ctrl Pts',(14.8743203079702,-9.,305.389849883143));
#2031=CARTESIAN_POINT('Ctrl Pts',(14.7151010160305,-9.,299.547166753218));
#2032=CARTESIAN_POINT('Ctrl Pts',(14.3613339472215,-9.,293.114195242939));
#2033=CARTESIAN_POINT('Ctrl Pts',(12.5329121501934,-9.,288.887907445925));
#2034=CARTESIAN_POINT('Ctrl Pts',(11.3428854490917,-9.,286.13723179047));
#2035=CARTESIAN_POINT('Ctrl Pts',(9.62598372131269,-9.,284.320800585332));
#2036=CARTESIAN_POINT('Ctrl Pts',(6.96718239188881,-9.,283.179505866003));
#2037=CARTESIAN_POINT('Ctrl Pts',(5.58089918248363,-9.,282.584441583133));
#2038=CARTESIAN_POINT('Ctrl Pts',(3.92777602497513,-9.,282.18420900116));
#2039=CARTESIAN_POINT('Ctrl Pts',(1.99999999999782,-9.,282.007690234858));
#2040=CARTESIAN_POINT('Ctrl Pts',(1.94431052069477,-9.,282.002590971222));
#2041=CARTESIAN_POINT('Ctrl Pts',(1.88839473154122,-9.,281.99767827841));
#2042=CARTESIAN_POINT('Ctrl Pts',(1.8322528584517,-9.,281.992952808398));
#2043=CARTESIAN_POINT('Ctrl Pts',(1.22150190563442,-9.,281.941545807639));
#2044=CARTESIAN_POINT('Ctrl Pts',(0.610750952817164,-9.,281.890138806881));
#2045=CARTESIAN_POINT('Ctrl Pts',(-8.59312621059871E-14,-9.,281.838731806122));
#2046=CARTESIAN_POINT('Ctrl Pts',(17.,-9.,316.));
#2047=CARTESIAN_POINT('Ctrl Pts',(17.,12.6,316.));
#2048=CARTESIAN_POINT('Ctrl Pts',(17.,-9.,315.50441646936));
#2049=CARTESIAN_POINT('Ctrl Pts',(17.,12.6,315.50441646936));
#2050=CARTESIAN_POINT('Ctrl Pts',(16.9985513080952,-9.,314.491917916066));
#2051=CARTESIAN_POINT('Ctrl Pts',(16.9985513080952,12.6,314.491917916066));
#2052=CARTESIAN_POINT('Ctrl Pts',(16.9920318646118,-9.,312.909176752281));
#2053=CARTESIAN_POINT('Ctrl Pts',(16.9920318646118,12.6,312.909176752281));
#2054=CARTESIAN_POINT('Ctrl Pts',(16.9745170477256,-9.,310.674187150777));
#2055=CARTESIAN_POINT('Ctrl Pts',(16.9745170477256,12.6,310.674187150777));
#2056=CARTESIAN_POINT('Ctrl Pts',(16.9338349467122,-9.,307.69587590639));
#2057=CARTESIAN_POINT('Ctrl Pts',(16.9338349467122,12.6,307.69587590639));
#2058=CARTESIAN_POINT('Ctrl Pts',(16.8634487703245,-9.,304.57015716772));
#2059=CARTESIAN_POINT('Ctrl Pts',(16.8634487703245,12.6,304.57015716772));
#2060=CARTESIAN_POINT('Ctrl Pts',(16.7422790149997,-9.,301.348120547886));
#2061=CARTESIAN_POINT('Ctrl Pts',(16.7422790149997,12.6,301.348120547886));
#2062=CARTESIAN_POINT('Ctrl Pts',(16.5359735439045,-9.,298.095070696299));
#2063=CARTESIAN_POINT('Ctrl Pts',(16.5359735439045,12.6,298.095070696299));
#2064=CARTESIAN_POINT('Ctrl Pts',(16.1926929497518,-9.,294.892205598351));
#2065=CARTESIAN_POINT('Ctrl Pts',(16.1926929497518,12.6,294.892205598351));
#2066=CARTESIAN_POINT('Ctrl Pts',(15.6496061172615,-9.,291.82914277586));
#2067=CARTESIAN_POINT('Ctrl Pts',(15.6496061172615,12.6,291.82914277586));
#2068=CARTESIAN_POINT('Ctrl Pts',(14.8403951587419,-9.,288.995763819941));
#2069=CARTESIAN_POINT('Ctrl Pts',(14.8403951587419,12.6,288.995763819941));
#2070=CARTESIAN_POINT('Ctrl Pts',(13.7033484644208,-9.,286.473438815185));
#2071=CARTESIAN_POINT('Ctrl Pts',(13.7033484644208,12.6,286.473438815185));
#2072=CARTESIAN_POINT('Ctrl Pts',(12.1890242800701,-9.,284.326851421562));
#2073=CARTESIAN_POINT('Ctrl Pts',(12.1890242800701,12.6,284.326851421562));
#2074=CARTESIAN_POINT('Ctrl Pts',(10.2723403348262,-9.,282.590975648728));
#2075=CARTESIAN_POINT('Ctrl Pts',(10.2723403348262,12.6,282.590975648728));
#2076=CARTESIAN_POINT('Ctrl Pts',(7.94806288019228,-9.,281.276448102944));
#2077=CARTESIAN_POINT('Ctrl Pts',(7.94806288019228,12.6,281.276448102944));
#2078=CARTESIAN_POINT('Ctrl Pts',(5.76616670029465,-9.,280.560219196132));
#2079=CARTESIAN_POINT('Ctrl Pts',(5.76616670029465,12.6,280.560219196132));
#2080=CARTESIAN_POINT('Ctrl Pts',(3.9517913938126,-9.,280.208504145521));
#2081=CARTESIAN_POINT('Ctrl Pts',(3.9517913938126,12.6,280.208504145521));
#2082=CARTESIAN_POINT('Ctrl Pts',(2.66368424066569,-9.,280.055862403662));
#2083=CARTESIAN_POINT('Ctrl Pts',(2.66368424066569,12.6,280.055862403662));
#2084=CARTESIAN_POINT('Ctrl Pts',(2.,-9.,280.));
#2085=CARTESIAN_POINT('Ctrl Pts',(2.,12.6,280.));
#2086=CARTESIAN_POINT('Ctrl Pts',(1.,-9.,279.91582984763));
#2087=CARTESIAN_POINT('Ctrl Pts',(1.,12.6,279.91582984763));
#2088=CARTESIAN_POINT('Ctrl Pts',(-1.11022302462516E-15,-9.,279.831659695261));
#2089=CARTESIAN_POINT('Ctrl Pts',(-1.11022302462516E-15,12.6,279.831659695261));
#2090=CARTESIAN_POINT('Ctrl Pts',(-1.,-9.,279.747489542891));
#2091=CARTESIAN_POINT('Ctrl Pts',(-1.,12.6,279.747489542891));
#2092=CARTESIAN_POINT('Ctrl Pts',(-2.,-9.,279.663319390522));
#2093=CARTESIAN_POINT('Ctrl Pts',(-2.,12.6,279.663319390522));
#2094=CARTESIAN_POINT('Ctrl Pts',(-3.,-9.,279.579149238152));
#2095=CARTESIAN_POINT('Ctrl Pts',(-3.,12.6,279.579149238152));
#2096=CARTESIAN_POINT('',(17.,0.,316.));
#2097=CARTESIAN_POINT('Origin',(17.,0.,324.));
#2098=CARTESIAN_POINT('',(17.,0.,324.));
#2099=CARTESIAN_POINT('Origin',(15.,0.,324.));
#2100=CARTESIAN_POINT('',(15.,0.,324.));
#2101=CARTESIAN_POINT('Origin',(15.,0.,316.));
#2102=CARTESIAN_POINT('',(15.,0.,316.));
#2103=CARTESIAN_POINT('Ctrl Pts',(-3.46055768059205,-9.01917151683795,281.547456138864));
#2104=CARTESIAN_POINT('Ctrl Pts',(-3.46055768059205,12.6038343033676,281.547456138864));
#2105=CARTESIAN_POINT('Ctrl Pts',(-1.69628750091079,-9.01917151683795,281.695955028708));
#2106=CARTESIAN_POINT('Ctrl Pts',(-1.69628750091079,12.6038343033676,281.695955028708));
#2107=CARTESIAN_POINT('Ctrl Pts',(0.0679826787703758,-9.01917151683795,
281.844453918553));
#2108=CARTESIAN_POINT('Ctrl Pts',(0.0679826787703758,12.6038343033676,281.844453918553));
#2109=CARTESIAN_POINT('Ctrl Pts',(1.8322528584517,-9.01917151683795,281.992952808398));
#2110=CARTESIAN_POINT('Ctrl Pts',(1.8322528584517,12.6038343033676,281.992952808398));
#2111=CARTESIAN_POINT('Ctrl Pts',(1.88839473154122,-9.01917151683795,281.99767827841));
#2112=CARTESIAN_POINT('Ctrl Pts',(1.88839473154122,12.6038343033676,281.99767827841));
#2113=CARTESIAN_POINT('Ctrl Pts',(1.94431052069477,-9.01917151683795,282.002590971222));
#2114=CARTESIAN_POINT('Ctrl Pts',(1.94431052069477,12.6038343033676,282.002590971222));
#2115=CARTESIAN_POINT('Ctrl Pts',(1.99999999999782,-9.01917151683795,282.007690234858));
#2116=CARTESIAN_POINT('Ctrl Pts',(1.99999999999782,12.6038343033676,282.007690234858));
#2117=CARTESIAN_POINT('Ctrl Pts',(3.92777602497513,-9.01917151683795,282.18420900116));
#2118=CARTESIAN_POINT('Ctrl Pts',(3.92777602497513,12.6038343033676,282.18420900116));
#2119=CARTESIAN_POINT('Ctrl Pts',(5.58089918248363,-9.01917151683795,282.584441583133));
#2120=CARTESIAN_POINT('Ctrl Pts',(5.58089918248363,12.6038343033676,282.584441583133));
#2121=CARTESIAN_POINT('Ctrl Pts',(6.96718239188881,-9.01917151683795,283.179505866003));
#2122=CARTESIAN_POINT('Ctrl Pts',(6.96718239188881,12.6038343033676,283.179505866003));
#2123=CARTESIAN_POINT('Ctrl Pts',(9.62598372131269,-9.01917151683795,284.320800585332));
#2124=CARTESIAN_POINT('Ctrl Pts',(9.62598372131269,12.6038343033676,284.320800585332));
#2125=CARTESIAN_POINT('Ctrl Pts',(11.3428854490917,-9.01917151683795,286.13723179047));
#2126=CARTESIAN_POINT('Ctrl Pts',(11.3428854490917,12.6038343033676,286.13723179047));
#2127=CARTESIAN_POINT('Ctrl Pts',(12.5329121501934,-9.01917151683795,288.887907445925));
#2128=CARTESIAN_POINT('Ctrl Pts',(12.5329121501934,12.6038343033676,288.887907445925));
#2129=CARTESIAN_POINT('Ctrl Pts',(14.3613339472215,-9.01917151683795,293.114195242939));
#2130=CARTESIAN_POINT('Ctrl Pts',(14.3613339472215,12.6038343033676,293.114195242939));
#2131=CARTESIAN_POINT('Ctrl Pts',(14.7151010160305,-9.01917151683795,299.547166753218));
#2132=CARTESIAN_POINT('Ctrl Pts',(14.7151010160305,12.6038343033676,299.547166753218));
#2133=CARTESIAN_POINT('Ctrl Pts',(14.8743203079702,-9.01917151683795,305.389849883143));
#2134=CARTESIAN_POINT('Ctrl Pts',(14.8743203079702,12.6038343033676,305.389849883143));
#2135=CARTESIAN_POINT('Ctrl Pts',(14.9804665025967,-9.01917151683795,309.284971969759));
#2136=CARTESIAN_POINT('Ctrl Pts',(14.9804665025967,12.6038343033676,309.284971969759));
#2137=CARTESIAN_POINT('Ctrl Pts',(15.,-9.01917151683795,312.917218954967));
#2138=CARTESIAN_POINT('Ctrl Pts',(15.,12.6038343033676,312.917218954967));
#2139=CARTESIAN_POINT('Ctrl Pts',(15.,-9.01917151683795,316.));
#2140=CARTESIAN_POINT('Ctrl Pts',(15.,12.6038343033676,316.));
#2141=CARTESIAN_POINT('',(0.,0.,0.));
#2142=CARTESIAN_POINT('Ctrl Pts',(-27.,1.99568395523348E-13,320.5));
#2143=CARTESIAN_POINT('Ctrl Pts',(-27.,-0.499999999999559,320.5));
#2144=CARTESIAN_POINT('Ctrl Pts',(-27.,-0.499999999999559,320.));
#2145=CARTESIAN_POINT('Ctrl Pts',(-27.,-0.499999999999559,319.5));
#2146=CARTESIAN_POINT('Ctrl Pts',(-27.,1.99568395523348E-13,319.5));
#2147=CARTESIAN_POINT('Ctrl Pts',(-27.,0.499999999999958,319.5));
#2148=CARTESIAN_POINT('Ctrl Pts',(-27.,0.499999999999958,320.));
#2149=CARTESIAN_POINT('Ctrl Pts',(-26.9999999999999,0.499999999999958,320.5));
#2150=CARTESIAN_POINT('Ctrl Pts',(-27.,1.99568395523348E-13,320.5));
#2151=CARTESIAN_POINT('Ctrl Pts',(-27.0000000000002,1.99568395523362E-13,
324.));
#2152=CARTESIAN_POINT('Ctrl Pts',(-27.0000000000004,-4.00000000000003,324.));
#2153=CARTESIAN_POINT('Ctrl Pts',(-27.0000000000004,-4.00000000000003,320.));
#2154=CARTESIAN_POINT('Ctrl Pts',(-27.0000000000005,-4.00000000000003,316.));
#2155=CARTESIAN_POINT('Ctrl Pts',(-27.0000000000003,1.99568395523362E-13,
316.));
#2156=CARTESIAN_POINT('Ctrl Pts',(-27.0000000000001,4.00000000000043,316.));
#2157=CARTESIAN_POINT('Ctrl Pts',(-27.,4.00000000000043,320.));
#2158=CARTESIAN_POINT('Ctrl Pts',(-27.,4.00000000000043,324.));
#2159=CARTESIAN_POINT('Ctrl Pts',(-27.0000000000002,1.99568395523362E-13,
324.));
#2160=CARTESIAN_POINT('Ctrl Pts',(-23.4999999999997,2.05109366990699E-14,
324.));
#2161=CARTESIAN_POINT('Ctrl Pts',(-23.4999999999999,-3.99999999999996,324.));
#2162=CARTESIAN_POINT('Ctrl Pts',(-23.5,-3.99999999999997,320.));
#2163=CARTESIAN_POINT('Ctrl Pts',(-23.5,-3.99999999999996,316.));
#2164=CARTESIAN_POINT('Ctrl Pts',(-23.4999999999998,2.05109366990698E-14,
316.));
#2165=CARTESIAN_POINT('Ctrl Pts',(-23.4999999999996,4.00000000000001,316.));
#2166=CARTESIAN_POINT('Ctrl Pts',(-23.4999999999996,4.00000000000001,320.));
#2167=CARTESIAN_POINT('Ctrl Pts',(-23.4999999999995,4.00000000000001,324.));
#2168=CARTESIAN_POINT('Ctrl Pts',(-23.4999999999997,2.05109366990699E-14,
324.));
#2169=CARTESIAN_POINT('',(-23.5,-3.99999999999999,320.));
#2170=CARTESIAN_POINT('',(-23.5,2.00210779794253E-14,324.));
#2171=CARTESIAN_POINT('Origin',(-23.5,0.,320.));
#2172=CARTESIAN_POINT('Origin',(-23.5,0.,320.));
#2173=CARTESIAN_POINT('',(-27.,-6.12323399573687E-17,320.5));
#2174=CARTESIAN_POINT('Origin',(-23.5,2.04497043591234E-14,320.5));
#2175=CARTESIAN_POINT('Origin',(-27.,0.,320.));
#2176=CARTESIAN_POINT('Origin',(-2.,0.,320.));
#2177=CARTESIAN_POINT('',(-17.,-3.99999999999999,320.));
#2178=CARTESIAN_POINT('Origin',(-17.,0.,320.));
#2179=CARTESIAN_POINT('',(-2.,-3.99999999999999,320.));
#2180=CARTESIAN_POINT('Origin',(-27.,0.,320.));
#2181=CARTESIAN_POINT('Origin',(-17.,0.,320.));
#2182=CARTESIAN_POINT('',(0.,0.,0.));
#2183=CARTESIAN_POINT('Ctrl Pts',(-24.9999999999999,1.38434137533096E-13,
180.5));
#2184=CARTESIAN_POINT('Ctrl Pts',(-24.9999999999999,-0.499999999999194,
180.5));
#2185=CARTESIAN_POINT('Ctrl Pts',(-25.,-0.499999999999194,180.000000000001));
#2186=CARTESIAN_POINT('Ctrl Pts',(-25.0000000000001,-0.499999999999194,
179.500000000001));
#2187=CARTESIAN_POINT('Ctrl Pts',(-25.0000000000001,1.38434137533096E-13,
179.500000000001));
#2188=CARTESIAN_POINT('Ctrl Pts',(-25.0000000000001,0.49999999999947,179.500000000001));
#2189=CARTESIAN_POINT('Ctrl Pts',(-25.,0.499999999999471,180.000000000001));
#2190=CARTESIAN_POINT('Ctrl Pts',(-24.9999999999999,0.49999999999947,180.5));
#2191=CARTESIAN_POINT('Ctrl Pts',(-24.9999999999999,1.38434137533096E-13,
180.5));
#2192=CARTESIAN_POINT('Ctrl Pts',(-25.0000000000001,1.38434137533119E-13,
184.000000000001));
#2193=CARTESIAN_POINT('Ctrl Pts',(-25.0000000000002,-4.00000000000052,184.000000000001));
#2194=CARTESIAN_POINT('Ctrl Pts',(-25.0000000000008,-4.00000000000052,180.000000000001));
#2195=CARTESIAN_POINT('Ctrl Pts',(-25.0000000000014,-4.00000000000052,176.));
#2196=CARTESIAN_POINT('Ctrl Pts',(-25.0000000000013,1.38434137533119E-13,
176.));
#2197=CARTESIAN_POINT('Ctrl Pts',(-25.0000000000011,4.0000000000008,176.));
#2198=CARTESIAN_POINT('Ctrl Pts',(-25.0000000000005,4.0000000000008,180.000000000001));
#2199=CARTESIAN_POINT('Ctrl Pts',(-25.,4.0000000000008,184.000000000001));
#2200=CARTESIAN_POINT('Ctrl Pts',(-25.0000000000001,1.38434137533119E-13,
184.000000000001));
#2201=CARTESIAN_POINT('Ctrl Pts',(-21.4999999999988,1.86764666232119E-14,
184.));
#2202=CARTESIAN_POINT('Ctrl Pts',(-21.4999999999989,-3.99999999999997,184.));
#2203=CARTESIAN_POINT('Ctrl Pts',(-21.4999999999995,-3.99999999999997,180.));
#2204=CARTESIAN_POINT('Ctrl Pts',(-21.5000000000001,-3.99999999999997,176.));
#2205=CARTESIAN_POINT('Ctrl Pts',(-21.5,1.86764666232117E-14,176.));
#2206=CARTESIAN_POINT('Ctrl Pts',(-21.4999999999998,4.,176.));
#2207=CARTESIAN_POINT('Ctrl Pts',(-21.4999999999992,4.,180.));
#2208=CARTESIAN_POINT('Ctrl Pts',(-21.4999999999986,4.,184.));
#2209=CARTESIAN_POINT('Ctrl Pts',(-21.4999999999988,1.86764666232119E-14,
184.));
#2210=CARTESIAN_POINT('',(-21.5,-3.99999999999999,180.));
#2211=CARTESIAN_POINT('',(-21.5,1.81866079035945E-14,184.));
#2212=CARTESIAN_POINT('Origin',(-21.5,0.,180.));
#2213=CARTESIAN_POINT('Origin',(-21.5,0.,180.));
#2214=CARTESIAN_POINT('',(-25.,-6.12323399573644E-17,180.5));
#2215=CARTESIAN_POINT('Origin',(-21.5,1.86152342832779E-14,180.5));
#2216=CARTESIAN_POINT('Origin',(-25.,0.,180.));
#2217=CARTESIAN_POINT('Origin',(0.,0.,180.));
#2218=CARTESIAN_POINT('',(-15.,-3.99999999999999,180.));
#2219=CARTESIAN_POINT('Origin',(-15.,0.,180.));
#2220=CARTESIAN_POINT('',(0.,-3.99999999999999,180.));
#2221=CARTESIAN_POINT('Origin',(-25.,0.,180.));
#2222=CARTESIAN_POINT('Origin',(-15.,0.,180.));
#2223=CARTESIAN_POINT('',(0.,0.,0.));
#2224=CARTESIAN_POINT('Ctrl Pts',(23.4999999999997,2.05109366990699E-14,
324.));
#2225=CARTESIAN_POINT('Ctrl Pts',(23.4999999999999,-3.99999999999996,324.));
#2226=CARTESIAN_POINT('Ctrl Pts',(23.5,-3.99999999999997,320.));
#2227=CARTESIAN_POINT('Ctrl Pts',(23.5,-3.99999999999996,316.));
#2228=CARTESIAN_POINT('Ctrl Pts',(23.4999999999998,2.05109366990698E-14,
316.));
#2229=CARTESIAN_POINT('Ctrl Pts',(23.4999999999996,4.00000000000001,316.));
#2230=CARTESIAN_POINT('Ctrl Pts',(23.4999999999996,4.00000000000001,320.));
#2231=CARTESIAN_POINT('Ctrl Pts',(23.4999999999995,4.00000000000001,324.));
#2232=CARTESIAN_POINT('Ctrl Pts',(23.4999999999997,2.05109366990699E-14,
324.));
#2233=CARTESIAN_POINT('Ctrl Pts',(27.0000000000002,1.99568395523362E-13,
324.));
#2234=CARTESIAN_POINT('Ctrl Pts',(27.0000000000004,-4.00000000000003,324.));
#2235=CARTESIAN_POINT('Ctrl Pts',(27.0000000000004,-4.00000000000003,320.));
#2236=CARTESIAN_POINT('Ctrl Pts',(27.0000000000005,-4.00000000000003,316.));
#2237=CARTESIAN_POINT('Ctrl Pts',(27.0000000000003,1.99568395523362E-13,
316.));
#2238=CARTESIAN_POINT('Ctrl Pts',(27.0000000000001,4.00000000000043,316.));
#2239=CARTESIAN_POINT('Ctrl Pts',(27.,4.00000000000043,320.));
#2240=CARTESIAN_POINT('Ctrl Pts',(27.,4.00000000000043,324.));
#2241=CARTESIAN_POINT('Ctrl Pts',(27.0000000000002,1.99568395523362E-13,
324.));
#2242=CARTESIAN_POINT('Ctrl Pts',(27.,1.99568395523348E-13,320.5));
#2243=CARTESIAN_POINT('Ctrl Pts',(27.,-0.499999999999559,320.5));
#2244=CARTESIAN_POINT('Ctrl Pts',(27.,-0.499999999999559,320.));
#2245=CARTESIAN_POINT('Ctrl Pts',(27.,-0.499999999999559,319.5));
#2246=CARTESIAN_POINT('Ctrl Pts',(27.,1.99568395523348E-13,319.5));
#2247=CARTESIAN_POINT('Ctrl Pts',(27.,0.499999999999958,319.5));
#2248=CARTESIAN_POINT('Ctrl Pts',(27.,0.499999999999958,320.));
#2249=CARTESIAN_POINT('Ctrl Pts',(26.9999999999999,0.499999999999958,320.5));
#2250=CARTESIAN_POINT('Ctrl Pts',(27.,1.99568395523348E-13,320.5));
#2251=CARTESIAN_POINT('',(23.5,-3.99999999999999,320.));
#2252=CARTESIAN_POINT('',(23.5,2.00210779794253E-14,324.));
#2253=CARTESIAN_POINT('Origin',(23.5,0.,320.));
#2254=CARTESIAN_POINT('',(27.,-6.12323399573687E-17,320.5));
#2255=CARTESIAN_POINT('Origin',(23.5,2.04497043591234E-14,320.5));
#2256=CARTESIAN_POINT('Origin',(27.,0.,320.));
#2257=CARTESIAN_POINT('Origin',(23.5,0.,320.));
#2258=CARTESIAN_POINT('Origin',(2.,0.,320.));
#2259=CARTESIAN_POINT('',(17.,-3.99999999999999,320.));
#2260=CARTESIAN_POINT('',(2.,-3.99999999999999,320.));
#2261=CARTESIAN_POINT('Origin',(17.,0.,320.));
#2262=CARTESIAN_POINT('Origin',(27.,0.,320.));
#2263=CARTESIAN_POINT('Origin',(17.,0.,320.));
#2264=CARTESIAN_POINT('',(0.,0.,0.));
#2265=CARTESIAN_POINT('Origin',(0.,-9.,162.));
#2266=CARTESIAN_POINT('',(-15.,-9.,184.));
#2267=CARTESIAN_POINT('',(-15.,-9.,176.));
#2268=CARTESIAN_POINT('',(-15.,-9.,184.));
#2269=CARTESIAN_POINT('',(0.,-9.,140.));
#2270=CARTESIAN_POINT('Ctrl Pts',(-15.,-9.,176.));
#2271=CARTESIAN_POINT('Ctrl Pts',(-15.,-9.,175.50441646936));
#2272=CARTESIAN_POINT('Ctrl Pts',(-14.9985513080952,-9.,174.491917916066));
#2273=CARTESIAN_POINT('Ctrl Pts',(-14.9920318646118,-9.,172.909176752281));
#2274=CARTESIAN_POINT('Ctrl Pts',(-14.9745170477256,-9.,170.674187150777));
#2275=CARTESIAN_POINT('Ctrl Pts',(-14.9338349467122,-9.,167.69587590639));
#2276=CARTESIAN_POINT('Ctrl Pts',(-14.8634487703245,-9.,164.57015716772));
#2277=CARTESIAN_POINT('Ctrl Pts',(-14.7422790149997,-9.,161.348120547886));
#2278=CARTESIAN_POINT('Ctrl Pts',(-14.5359735439045,-9.,158.095070696299));
#2279=CARTESIAN_POINT('Ctrl Pts',(-14.1926929497518,-9.,154.892205598351));
#2280=CARTESIAN_POINT('Ctrl Pts',(-13.6496061172615,-9.,151.82914277586));
#2281=CARTESIAN_POINT('Ctrl Pts',(-12.8403951587419,-9.,148.995763819941));
#2282=CARTESIAN_POINT('Ctrl Pts',(-11.7033484644208,-9.,146.473438815185));
#2283=CARTESIAN_POINT('Ctrl Pts',(-10.1890242800701,-9.,144.326851421562));
#2284=CARTESIAN_POINT('Ctrl Pts',(-8.27234033482616,-9.,142.590975648728));
#2285=CARTESIAN_POINT('Ctrl Pts',(-5.94806288019228,-9.,141.276448102944));
#2286=CARTESIAN_POINT('Ctrl Pts',(-3.76616670029465,-9.,140.560219196132));
#2287=CARTESIAN_POINT('Ctrl Pts',(-1.9517913938126,-9.,140.208504145521));
#2288=CARTESIAN_POINT('Ctrl Pts',(-0.663684240665688,-9.,140.055862403662));
#2289=CARTESIAN_POINT('Ctrl Pts',(0.,-9.,140.));
#2290=CARTESIAN_POINT('',(15.,-9.,176.));
#2291=CARTESIAN_POINT('Ctrl Pts',(0.,-9.,140.));
#2292=CARTESIAN_POINT('Ctrl Pts',(0.663684240665688,-9.,140.055862403662));
#2293=CARTESIAN_POINT('Ctrl Pts',(1.9517913938126,-9.,140.208504145521));
#2294=CARTESIAN_POINT('Ctrl Pts',(3.76616670029465,-9.,140.560219196132));
#2295=CARTESIAN_POINT('Ctrl Pts',(5.94806288019228,-9.,141.276448102944));
#2296=CARTESIAN_POINT('Ctrl Pts',(8.27234033482616,-9.,142.590975648728));
#2297=CARTESIAN_POINT('Ctrl Pts',(10.1890242800701,-9.,144.326851421562));
#2298=CARTESIAN_POINT('Ctrl Pts',(11.7033484644208,-9.,146.473438815185));
#2299=CARTESIAN_POINT('Ctrl Pts',(12.8403951587419,-9.,148.995763819941));
#2300=CARTESIAN_POINT('Ctrl Pts',(13.6496061172615,-9.,151.82914277586));
#2301=CARTESIAN_POINT('Ctrl Pts',(14.1926929497518,-9.,154.892205598351));
#2302=CARTESIAN_POINT('Ctrl Pts',(14.5359735439045,-9.,158.095070696299));
#2303=CARTESIAN_POINT('Ctrl Pts',(14.7422790149997,-9.,161.348120547886));
#2304=CARTESIAN_POINT('Ctrl Pts',(14.8634487703245,-9.,164.57015716772));
#2305=CARTESIAN_POINT('Ctrl Pts',(14.9338349467122,-9.,167.69587590639));
#2306=CARTESIAN_POINT('Ctrl Pts',(14.9745170477256,-9.,170.674187150777));
#2307=CARTESIAN_POINT('Ctrl Pts',(14.9920318646118,-9.,172.909176752281));
#2308=CARTESIAN_POINT('Ctrl Pts',(14.9985513080952,-9.,174.491917916066));
#2309=CARTESIAN_POINT('Ctrl Pts',(15.,-9.,175.50441646936));
#2310=CARTESIAN_POINT('Ctrl Pts',(15.,-9.,176.));
#2311=CARTESIAN_POINT('',(15.,-9.,184.));
#2312=CARTESIAN_POINT('',(15.,-9.,184.));
#2313=CARTESIAN_POINT('',(13.,-9.,184.));
#2314=CARTESIAN_POINT('',(-15.,-9.,184.));
#2315=CARTESIAN_POINT('',(13.,-9.,176.));
#2316=CARTESIAN_POINT('',(13.,-9.,184.));
#2317=CARTESIAN_POINT('',(-2.28039809258007E-12,-9.,142.007690234858));
#2318=CARTESIAN_POINT('Ctrl Pts',(13.,-9.,176.));
#2319=CARTESIAN_POINT('Ctrl Pts',(13.,-9.,172.917218954967));
#2320=CARTESIAN_POINT('Ctrl Pts',(12.9804665025967,-9.,169.284971969759));
#2321=CARTESIAN_POINT('Ctrl Pts',(12.7151010160305,-9.,159.547166753218));
#2322=CARTESIAN_POINT('Ctrl Pts',(12.3613339472215,-9.,153.114195242939));
#2323=CARTESIAN_POINT('Ctrl Pts',(9.34288544909169,-9.,146.13723179047));
#2324=CARTESIAN_POINT('Ctrl Pts',(7.62598372131269,-9.,144.320800585332));
#2325=CARTESIAN_POINT('Ctrl Pts',(3.58089918248363,-9.,142.584441583133));
#2326=CARTESIAN_POINT('Ctrl Pts',(1.92777602497513,-9.,142.18420900116));
#2327=CARTESIAN_POINT('Ctrl Pts',(-2.18252499406546E-12,-9.,142.007690234858));
#2328=CARTESIAN_POINT('',(-13.,-9.,176.));
#2329=CARTESIAN_POINT('Ctrl Pts',(-2.28102259303142E-12,-9.,142.007690234858));
#2330=CARTESIAN_POINT('Ctrl Pts',(-1.9277760249776,-9.,142.184209001161));
#2331=CARTESIAN_POINT('Ctrl Pts',(-3.58089918248474,-9.,142.584441583133));
#2332=CARTESIAN_POINT('Ctrl Pts',(-7.62598372131269,-9.,144.320800585332));
#2333=CARTESIAN_POINT('Ctrl Pts',(-9.34288544909169,-9.,146.13723179047));
#2334=CARTESIAN_POINT('Ctrl Pts',(-12.3613339472215,-9.,153.114195242939));
#2335=CARTESIAN_POINT('Ctrl Pts',(-12.7151010160305,-9.,159.547166753218));
#2336=CARTESIAN_POINT('Ctrl Pts',(-12.9804665025967,-9.,169.284971969759));
#2337=CARTESIAN_POINT('Ctrl Pts',(-13.,-9.,172.917218954967));
#2338=CARTESIAN_POINT('Ctrl Pts',(-13.,-9.,176.));
#2339=CARTESIAN_POINT('',(-13.,-9.,184.));
#2340=CARTESIAN_POINT('',(-13.,-9.,184.));
#2341=CARTESIAN_POINT('',(-15.,-9.,184.));
#2342=CARTESIAN_POINT('Ctrl Pts',(0.,-9.,140.));
#2343=CARTESIAN_POINT('Ctrl Pts',(0.,12.6,140.));
#2344=CARTESIAN_POINT('Ctrl Pts',(-0.663684240665688,-9.,140.055862403662));
#2345=CARTESIAN_POINT('Ctrl Pts',(-0.663684240665688,12.6,140.055862403662));
#2346=CARTESIAN_POINT('Ctrl Pts',(-1.9517913938126,-9.,140.208504145521));
#2347=CARTESIAN_POINT('Ctrl Pts',(-1.9517913938126,12.6,140.208504145521));
#2348=CARTESIAN_POINT('Ctrl Pts',(-3.76616670029465,-9.,140.560219196132));
#2349=CARTESIAN_POINT('Ctrl Pts',(-3.76616670029465,12.6,140.560219196132));
#2350=CARTESIAN_POINT('Ctrl Pts',(-5.94806288019228,-9.,141.276448102944));
#2351=CARTESIAN_POINT('Ctrl Pts',(-5.94806288019228,12.6,141.276448102944));
#2352=CARTESIAN_POINT('Ctrl Pts',(-8.27234033482616,-9.,142.590975648728));
#2353=CARTESIAN_POINT('Ctrl Pts',(-8.27234033482616,12.6,142.590975648728));
#2354=CARTESIAN_POINT('Ctrl Pts',(-10.1890242800701,-9.,144.326851421562));
#2355=CARTESIAN_POINT('Ctrl Pts',(-10.1890242800701,12.6,144.326851421562));
#2356=CARTESIAN_POINT('Ctrl Pts',(-11.7033484644208,-9.,146.473438815185));
#2357=CARTESIAN_POINT('Ctrl Pts',(-11.7033484644208,12.6,146.473438815185));
#2358=CARTESIAN_POINT('Ctrl Pts',(-12.8403951587419,-9.,148.995763819941));
#2359=CARTESIAN_POINT('Ctrl Pts',(-12.8403951587419,12.6,148.995763819941));
#2360=CARTESIAN_POINT('Ctrl Pts',(-13.6496061172615,-9.,151.82914277586));
#2361=CARTESIAN_POINT('Ctrl Pts',(-13.6496061172615,12.6,151.82914277586));
#2362=CARTESIAN_POINT('Ctrl Pts',(-14.1926929497518,-9.,154.892205598351));
#2363=CARTESIAN_POINT('Ctrl Pts',(-14.1926929497518,12.6,154.892205598351));
#2364=CARTESIAN_POINT('Ctrl Pts',(-14.5359735439045,-9.,158.095070696299));
#2365=CARTESIAN_POINT('Ctrl Pts',(-14.5359735439045,12.6,158.095070696299));
#2366=CARTESIAN_POINT('Ctrl Pts',(-14.7422790149997,-9.,161.348120547886));
#2367=CARTESIAN_POINT('Ctrl Pts',(-14.7422790149997,12.6,161.348120547886));
#2368=CARTESIAN_POINT('Ctrl Pts',(-14.8634487703245,-9.,164.57015716772));
#2369=CARTESIAN_POINT('Ctrl Pts',(-14.8634487703245,12.6,164.57015716772));
#2370=CARTESIAN_POINT('Ctrl Pts',(-14.9338349467122,-9.,167.69587590639));
#2371=CARTESIAN_POINT('Ctrl Pts',(-14.9338349467122,12.6,167.69587590639));
#2372=CARTESIAN_POINT('Ctrl Pts',(-14.9745170477256,-9.,170.674187150777));
#2373=CARTESIAN_POINT('Ctrl Pts',(-14.9745170477256,12.6,170.674187150777));
#2374=CARTESIAN_POINT('Ctrl Pts',(-14.9920318646118,-9.,172.909176752281));
#2375=CARTESIAN_POINT('Ctrl Pts',(-14.9920318646118,12.6,172.909176752281));
#2376=CARTESIAN_POINT('Ctrl Pts',(-14.9985513080952,-9.,174.491917916066));
#2377=CARTESIAN_POINT('Ctrl Pts',(-14.9985513080952,12.6,174.491917916066));
#2378=CARTESIAN_POINT('Ctrl Pts',(-15.,-9.,175.50441646936));
#2379=CARTESIAN_POINT('Ctrl Pts',(-15.,12.6,175.50441646936));
#2380=CARTESIAN_POINT('Ctrl Pts',(-15.,-9.,176.));
#2381=CARTESIAN_POINT('Ctrl Pts',(-15.,12.6,176.));
#2382=CARTESIAN_POINT('',(-15.,9.,176.));
#2383=CARTESIAN_POINT('',(-15.,0.,176.));
#2384=CARTESIAN_POINT('',(0.,9.,140.));
#2385=CARTESIAN_POINT('Ctrl Pts',(0.,9.,140.));
#2386=CARTESIAN_POINT('Ctrl Pts',(-0.663684240665688,9.,140.055862403662));
#2387=CARTESIAN_POINT('Ctrl Pts',(-1.9517913938126,9.,140.208504145521));
#2388=CARTESIAN_POINT('Ctrl Pts',(-3.76616670029465,9.,140.560219196132));
#2389=CARTESIAN_POINT('Ctrl Pts',(-5.94806288019228,9.,141.276448102944));
#2390=CARTESIAN_POINT('Ctrl Pts',(-8.27234033482616,9.,142.590975648728));
#2391=CARTESIAN_POINT('Ctrl Pts',(-10.1890242800701,9.,144.326851421562));
#2392=CARTESIAN_POINT('Ctrl Pts',(-11.7033484644208,9.,146.473438815185));
#2393=CARTESIAN_POINT('Ctrl Pts',(-12.8403951587419,9.,148.995763819941));
#2394=CARTESIAN_POINT('Ctrl Pts',(-13.6496061172615,9.,151.82914277586));
#2395=CARTESIAN_POINT('Ctrl Pts',(-14.1926929497518,9.,154.892205598351));
#2396=CARTESIAN_POINT('Ctrl Pts',(-14.5359735439045,9.,158.095070696299));
#2397=CARTESIAN_POINT('Ctrl Pts',(-14.7422790149997,9.,161.348120547886));
#2398=CARTESIAN_POINT('Ctrl Pts',(-14.8634487703245,9.,164.57015716772));
#2399=CARTESIAN_POINT('Ctrl Pts',(-14.9338349467122,9.,167.69587590639));
#2400=CARTESIAN_POINT('Ctrl Pts',(-14.9745170477256,9.,170.674187150777));
#2401=CARTESIAN_POINT('Ctrl Pts',(-14.9920318646118,9.,172.909176752281));
#2402=CARTESIAN_POINT('Ctrl Pts',(-14.9985513080952,9.,174.491917916066));
#2403=CARTESIAN_POINT('Ctrl Pts',(-15.,9.,175.50441646936));
#2404=CARTESIAN_POINT('Ctrl Pts',(-15.,9.,176.));
#2405=CARTESIAN_POINT('',(0.,0.,140.));
#2406=CARTESIAN_POINT('Ctrl Pts',(15.,-9.,176.));
#2407=CARTESIAN_POINT('Ctrl Pts',(15.,12.6,176.));
#2408=CARTESIAN_POINT('Ctrl Pts',(15.,-9.,175.50441646936));
#2409=CARTESIAN_POINT('Ctrl Pts',(15.,12.6,175.50441646936));
#2410=CARTESIAN_POINT('Ctrl Pts',(14.9985513080952,-9.,174.491917916066));
#2411=CARTESIAN_POINT('Ctrl Pts',(14.9985513080952,12.6,174.491917916066));
#2412=CARTESIAN_POINT('Ctrl Pts',(14.9920318646118,-9.,172.909176752281));
#2413=CARTESIAN_POINT('Ctrl Pts',(14.9920318646118,12.6,172.909176752281));
#2414=CARTESIAN_POINT('Ctrl Pts',(14.9745170477256,-9.,170.674187150777));
#2415=CARTESIAN_POINT('Ctrl Pts',(14.9745170477256,12.6,170.674187150777));
#2416=CARTESIAN_POINT('Ctrl Pts',(14.9338349467122,-9.,167.69587590639));
#2417=CARTESIAN_POINT('Ctrl Pts',(14.9338349467122,12.6,167.69587590639));
#2418=CARTESIAN_POINT('Ctrl Pts',(14.8634487703245,-9.,164.57015716772));
#2419=CARTESIAN_POINT('Ctrl Pts',(14.8634487703245,12.6,164.57015716772));
#2420=CARTESIAN_POINT('Ctrl Pts',(14.7422790149997,-9.,161.348120547886));
#2421=CARTESIAN_POINT('Ctrl Pts',(14.7422790149997,12.6,161.348120547886));
#2422=CARTESIAN_POINT('Ctrl Pts',(14.5359735439045,-9.,158.095070696299));
#2423=CARTESIAN_POINT('Ctrl Pts',(14.5359735439045,12.6,158.095070696299));
#2424=CARTESIAN_POINT('Ctrl Pts',(14.1926929497518,-9.,154.892205598351));
#2425=CARTESIAN_POINT('Ctrl Pts',(14.1926929497518,12.6,154.892205598351));
#2426=CARTESIAN_POINT('Ctrl Pts',(13.6496061172615,-9.,151.82914277586));
#2427=CARTESIAN_POINT('Ctrl Pts',(13.6496061172615,12.6,151.82914277586));
#2428=CARTESIAN_POINT('Ctrl Pts',(12.8403951587419,-9.,148.995763819941));
#2429=CARTESIAN_POINT('Ctrl Pts',(12.8403951587419,12.6,148.995763819941));
#2430=CARTESIAN_POINT('Ctrl Pts',(11.7033484644208,-9.,146.473438815185));
#2431=CARTESIAN_POINT('Ctrl Pts',(11.7033484644208,12.6,146.473438815185));
#2432=CARTESIAN_POINT('Ctrl Pts',(10.1890242800701,-9.,144.326851421562));
#2433=CARTESIAN_POINT('Ctrl Pts',(10.1890242800701,12.6,144.326851421562));
#2434=CARTESIAN_POINT('Ctrl Pts',(8.27234033482616,-9.,142.590975648728));
#2435=CARTESIAN_POINT('Ctrl Pts',(8.27234033482616,12.6,142.590975648728));
#2436=CARTESIAN_POINT('Ctrl Pts',(5.94806288019228,-9.,141.276448102944));
#2437=CARTESIAN_POINT('Ctrl Pts',(5.94806288019228,12.6,141.276448102944));
#2438=CARTESIAN_POINT('Ctrl Pts',(3.76616670029465,-9.,140.560219196132));
#2439=CARTESIAN_POINT('Ctrl Pts',(3.76616670029465,12.6,140.560219196132));
#2440=CARTESIAN_POINT('Ctrl Pts',(1.9517913938126,-9.,140.208504145521));
#2441=CARTESIAN_POINT('Ctrl Pts',(1.9517913938126,12.6,140.208504145521));
#2442=CARTESIAN_POINT('Ctrl Pts',(0.663684240665688,-9.,140.055862403662));
#2443=CARTESIAN_POINT('Ctrl Pts',(0.663684240665688,12.6,140.055862403662));
#2444=CARTESIAN_POINT('Ctrl Pts',(0.,-9.,140.));
#2445=CARTESIAN_POINT('Ctrl Pts',(0.,12.6,140.));
#2446=CARTESIAN_POINT('',(15.,9.,176.));
#2447=CARTESIAN_POINT('Ctrl Pts',(15.,9.,176.));
#2448=CARTESIAN_POINT('Ctrl Pts',(15.,9.,175.50441646936));
#2449=CARTESIAN_POINT('Ctrl Pts',(14.9985513080952,9.,174.491917916066));
#2450=CARTESIAN_POINT('Ctrl Pts',(14.9920318646118,9.,172.909176752281));
#2451=CARTESIAN_POINT('Ctrl Pts',(14.9745170477256,9.,170.674187150777));
#2452=CARTESIAN_POINT('Ctrl Pts',(14.9338349467122,9.,167.69587590639));
#2453=CARTESIAN_POINT('Ctrl Pts',(14.8634487703245,9.,164.57015716772));
#2454=CARTESIAN_POINT('Ctrl Pts',(14.7422790149997,9.,161.348120547886));
#2455=CARTESIAN_POINT('Ctrl Pts',(14.5359735439045,9.,158.095070696299));
#2456=CARTESIAN_POINT('Ctrl Pts',(14.1926929497518,9.,154.892205598351));
#2457=CARTESIAN_POINT('Ctrl Pts',(13.6496061172615,9.,151.82914277586));
#2458=CARTESIAN_POINT('Ctrl Pts',(12.8403951587419,9.,148.995763819941));
#2459=CARTESIAN_POINT('Ctrl Pts',(11.7033484644208,9.,146.473438815185));
#2460=CARTESIAN_POINT('Ctrl Pts',(10.1890242800701,9.,144.326851421562));
#2461=CARTESIAN_POINT('Ctrl Pts',(8.27234033482616,9.,142.590975648728));
#2462=CARTESIAN_POINT('Ctrl Pts',(5.94806288019228,9.,141.276448102944));
#2463=CARTESIAN_POINT('Ctrl Pts',(3.76616670029465,9.,140.560219196132));
#2464=CARTESIAN_POINT('Ctrl Pts',(1.9517913938126,9.,140.208504145521));
#2465=CARTESIAN_POINT('Ctrl Pts',(0.663684240665688,9.,140.055862403662));
#2466=CARTESIAN_POINT('Ctrl Pts',(0.,9.,140.));
#2467=CARTESIAN_POINT('',(15.,0.,176.));
#2468=CARTESIAN_POINT('Origin',(15.,0.,184.));
#2469=CARTESIAN_POINT('',(15.,9.,184.));
#2470=CARTESIAN_POINT('',(15.,9.,184.));
#2471=CARTESIAN_POINT('',(15.,0.,184.));
#2472=CARTESIAN_POINT('Origin',(13.,0.,184.));
#2473=CARTESIAN_POINT('',(13.,9.,184.));
#2474=CARTESIAN_POINT('',(-15.,9.,184.));
#2475=CARTESIAN_POINT('',(13.,0.,184.));
#2476=CARTESIAN_POINT('Origin',(13.,0.,176.));
#2477=CARTESIAN_POINT('',(13.,9.,176.));
#2478=CARTESIAN_POINT('',(13.,9.,184.));
#2479=CARTESIAN_POINT('',(13.,0.,176.));
#2480=CARTESIAN_POINT('Ctrl Pts',(-2.18252499406546E-12,-9.01917151683795,
142.007690234858));
#2481=CARTESIAN_POINT('Ctrl Pts',(-2.18252499406546E-12,12.6038343033676,
142.007690234858));
#2482=CARTESIAN_POINT('Ctrl Pts',(1.92777602497513,-9.01917151683795,142.18420900116));
#2483=CARTESIAN_POINT('Ctrl Pts',(1.92777602497513,12.6038343033676,142.18420900116));
#2484=CARTESIAN_POINT('Ctrl Pts',(3.58089918248363,-9.01917151683795,142.584441583133));
#2485=CARTESIAN_POINT('Ctrl Pts',(3.58089918248363,12.6038343033676,142.584441583133));
#2486=CARTESIAN_POINT('Ctrl Pts',(4.96718239188881,-9.01917151683795,143.179505866003));
#2487=CARTESIAN_POINT('Ctrl Pts',(4.96718239188881,12.6038343033676,143.179505866003));
#2488=CARTESIAN_POINT('Ctrl Pts',(7.62598372131269,-9.01917151683795,144.320800585332));
#2489=CARTESIAN_POINT('Ctrl Pts',(7.62598372131269,12.6038343033676,144.320800585332));
#2490=CARTESIAN_POINT('Ctrl Pts',(9.34288544909169,-9.01917151683795,146.13723179047));
#2491=CARTESIAN_POINT('Ctrl Pts',(9.34288544909169,12.6038343033676,146.13723179047));
#2492=CARTESIAN_POINT('Ctrl Pts',(10.5329121501934,-9.01917151683795,148.887907445925));
#2493=CARTESIAN_POINT('Ctrl Pts',(10.5329121501934,12.6038343033676,148.887907445925));
#2494=CARTESIAN_POINT('Ctrl Pts',(12.3613339472215,-9.01917151683795,153.114195242939));
#2495=CARTESIAN_POINT('Ctrl Pts',(12.3613339472215,12.6038343033676,153.114195242939));
#2496=CARTESIAN_POINT('Ctrl Pts',(12.7151010160305,-9.01917151683795,159.547166753218));
#2497=CARTESIAN_POINT('Ctrl Pts',(12.7151010160305,12.6038343033676,159.547166753218));
#2498=CARTESIAN_POINT('Ctrl Pts',(12.8743203079702,-9.01917151683795,165.389849883143));
#2499=CARTESIAN_POINT('Ctrl Pts',(12.8743203079702,12.6038343033676,165.389849883143));
#2500=CARTESIAN_POINT('Ctrl Pts',(12.9804665025967,-9.01917151683795,169.284971969759));
#2501=CARTESIAN_POINT('Ctrl Pts',(12.9804665025967,12.6038343033676,169.284971969759));
#2502=CARTESIAN_POINT('Ctrl Pts',(13.,-9.01917151683795,172.917218954967));
#2503=CARTESIAN_POINT('Ctrl Pts',(13.,12.6038343033676,172.917218954967));
#2504=CARTESIAN_POINT('Ctrl Pts',(13.,-9.01917151683795,176.));
#2505=CARTESIAN_POINT('Ctrl Pts',(13.,12.6038343033676,176.));
#2506=CARTESIAN_POINT('',(-2.28039809258007E-12,9.,142.007690234858));
#2507=CARTESIAN_POINT('Ctrl Pts',(-2.18252499406546E-12,9.,142.007690234858));
#2508=CARTESIAN_POINT('Ctrl Pts',(1.92777602497513,9.,142.18420900116));
#2509=CARTESIAN_POINT('Ctrl Pts',(3.58089918248363,9.,142.584441583133));
#2510=CARTESIAN_POINT('Ctrl Pts',(7.62598372131269,9.,144.320800585332));
#2511=CARTESIAN_POINT('Ctrl Pts',(9.34288544909169,9.,146.13723179047));
#2512=CARTESIAN_POINT('Ctrl Pts',(12.3613339472215,9.,153.114195242939));
#2513=CARTESIAN_POINT('Ctrl Pts',(12.7151010160305,9.,159.547166753218));
#2514=CARTESIAN_POINT('Ctrl Pts',(12.9804665025967,9.,169.284971969759));
#2515=CARTESIAN_POINT('Ctrl Pts',(13.,9.,172.917218954967));
#2516=CARTESIAN_POINT('Ctrl Pts',(13.,9.,176.));
#2517=CARTESIAN_POINT('',(-2.28102259303142E-12,0.,142.007690234858));
#2518=CARTESIAN_POINT('Ctrl Pts',(-13.,-9.01917151683795,176.));
#2519=CARTESIAN_POINT('Ctrl Pts',(-13.,12.6038343033676,176.));
#2520=CARTESIAN_POINT('Ctrl Pts',(-13.,-9.01917151683795,172.917218954967));
#2521=CARTESIAN_POINT('Ctrl Pts',(-13.,12.6038343033676,172.917218954967));
#2522=CARTESIAN_POINT('Ctrl Pts',(-12.9804665025967,-9.01917151683795,169.284971969759));
#2523=CARTESIAN_POINT('Ctrl Pts',(-12.9804665025967,12.6038343033676,169.284971969759));
#2524=CARTESIAN_POINT('Ctrl Pts',(-12.8743203079702,-9.01917151683795,165.389849883143));
#2525=CARTESIAN_POINT('Ctrl Pts',(-12.8743203079702,12.6038343033676,165.389849883143));
#2526=CARTESIAN_POINT('Ctrl Pts',(-12.7151010160305,-9.01917151683795,159.547166753218));
#2527=CARTESIAN_POINT('Ctrl Pts',(-12.7151010160305,12.6038343033676,159.547166753218));
#2528=CARTESIAN_POINT('Ctrl Pts',(-12.3613339472215,-9.01917151683795,153.114195242939));
#2529=CARTESIAN_POINT('Ctrl Pts',(-12.3613339472215,12.6038343033676,153.114195242939));
#2530=CARTESIAN_POINT('Ctrl Pts',(-10.5329121501934,-9.01917151683795,148.887907445925));
#2531=CARTESIAN_POINT('Ctrl Pts',(-10.5329121501934,12.6038343033676,148.887907445925));
#2532=CARTESIAN_POINT('Ctrl Pts',(-9.34288544909169,-9.01917151683795,146.13723179047));
#2533=CARTESIAN_POINT('Ctrl Pts',(-9.34288544909169,12.6038343033676,146.13723179047));
#2534=CARTESIAN_POINT('Ctrl Pts',(-7.62598372131269,-9.01917151683795,144.320800585332));
#2535=CARTESIAN_POINT('Ctrl Pts',(-7.62598372131269,12.6038343033676,144.320800585332));
#2536=CARTESIAN_POINT('Ctrl Pts',(-4.96718239188881,-9.01917151683795,143.179505866003));
#2537=CARTESIAN_POINT('Ctrl Pts',(-4.96718239188881,12.6038343033676,143.179505866003));
#2538=CARTESIAN_POINT('Ctrl Pts',(-3.58089918248474,-9.01917151683795,142.584441583133));
#2539=CARTESIAN_POINT('Ctrl Pts',(-3.58089918248474,12.6038343033676,142.584441583133));
#2540=CARTESIAN_POINT('Ctrl Pts',(-1.9277760249776,-9.01917151683795,142.184209001161));
#2541=CARTESIAN_POINT('Ctrl Pts',(-1.9277760249776,12.6038343033676,142.184209001161));
#2542=CARTESIAN_POINT('Ctrl Pts',(-2.28102259303142E-12,-9.01917151683795,
142.007690234858));
#2543=CARTESIAN_POINT('Ctrl Pts',(-2.28102259303142E-12,12.6038343033676,
142.007690234858));
#2544=CARTESIAN_POINT('',(-13.,9.,176.));
#2545=CARTESIAN_POINT('Ctrl Pts',(-13.,9.,176.));
#2546=CARTESIAN_POINT('Ctrl Pts',(-13.,9.,172.917218954967));
#2547=CARTESIAN_POINT('Ctrl Pts',(-12.9804665025967,9.,169.284971969759));
#2548=CARTESIAN_POINT('Ctrl Pts',(-12.7151010160305,9.,159.547166753218));
#2549=CARTESIAN_POINT('Ctrl Pts',(-12.3613339472215,9.,153.114195242939));
#2550=CARTESIAN_POINT('Ctrl Pts',(-9.34288544909169,9.,146.13723179047));
#2551=CARTESIAN_POINT('Ctrl Pts',(-7.62598372131269,9.,144.320800585332));
#2552=CARTESIAN_POINT('Ctrl Pts',(-3.58089918248474,9.,142.584441583133));
#2553=CARTESIAN_POINT('Ctrl Pts',(-1.9277760249776,9.,142.184209001161));
#2554=CARTESIAN_POINT('Ctrl Pts',(-2.28102259303142E-12,9.,142.007690234858));
#2555=CARTESIAN_POINT('',(-13.,0.,176.));
#2556=CARTESIAN_POINT('Origin',(-13.,0.,184.));
#2557=CARTESIAN_POINT('',(-13.,9.,184.));
#2558=CARTESIAN_POINT('',(-13.,9.,184.));
#2559=CARTESIAN_POINT('',(-13.,0.,184.));
#2560=CARTESIAN_POINT('Origin',(-15.,0.,184.));
#2561=CARTESIAN_POINT('',(-15.,9.,184.));
#2562=CARTESIAN_POINT('',(-15.,9.,184.));
#2563=CARTESIAN_POINT('',(-15.,0.,184.));
#2564=CARTESIAN_POINT('Origin',(-15.,0.,176.));
#2565=CARTESIAN_POINT('',(-15.,9.,184.));
#2566=CARTESIAN_POINT('Origin',(0.,9.,162.));
#2567=CARTESIAN_POINT('',(0.,0.,0.));
#2568=CARTESIAN_POINT('Ctrl Pts',(21.4999999999988,1.86764666232119E-14,
184.));
#2569=CARTESIAN_POINT('Ctrl Pts',(21.4999999999989,-3.99999999999997,184.));
#2570=CARTESIAN_POINT('Ctrl Pts',(21.4999999999995,-3.99999999999997,180.));
#2571=CARTESIAN_POINT('Ctrl Pts',(21.5000000000001,-3.99999999999997,176.));
#2572=CARTESIAN_POINT('Ctrl Pts',(21.5,1.86764666232117E-14,176.));
#2573=CARTESIAN_POINT('Ctrl Pts',(21.4999999999998,4.,176.));
#2574=CARTESIAN_POINT('Ctrl Pts',(21.4999999999992,4.,180.));
#2575=CARTESIAN_POINT('Ctrl Pts',(21.4999999999986,4.,184.));
#2576=CARTESIAN_POINT('Ctrl Pts',(21.4999999999988,1.86764666232119E-14,
184.));
#2577=CARTESIAN_POINT('Ctrl Pts',(25.0000000000001,1.38434137533119E-13,
184.000000000001));
#2578=CARTESIAN_POINT('Ctrl Pts',(25.0000000000002,-4.00000000000052,184.000000000001));
#2579=CARTESIAN_POINT('Ctrl Pts',(25.0000000000008,-4.00000000000052,180.000000000001));
#2580=CARTESIAN_POINT('Ctrl Pts',(25.0000000000014,-4.00000000000052,176.));
#2581=CARTESIAN_POINT('Ctrl Pts',(25.0000000000013,1.38434137533119E-13,
176.));
#2582=CARTESIAN_POINT('Ctrl Pts',(25.0000000000011,4.0000000000008,176.));
#2583=CARTESIAN_POINT('Ctrl Pts',(25.0000000000005,4.0000000000008,180.000000000001));
#2584=CARTESIAN_POINT('Ctrl Pts',(25.,4.0000000000008,184.000000000001));
#2585=CARTESIAN_POINT('Ctrl Pts',(25.0000000000001,1.38434137533119E-13,
184.000000000001));
#2586=CARTESIAN_POINT('Ctrl Pts',(24.9999999999999,1.38434137533096E-13,
180.5));
#2587=CARTESIAN_POINT('Ctrl Pts',(24.9999999999999,-0.499999999999194,180.5));
#2588=CARTESIAN_POINT('Ctrl Pts',(25.,-0.499999999999194,180.000000000001));
#2589=CARTESIAN_POINT('Ctrl Pts',(25.0000000000001,-0.499999999999194,179.500000000001));
#2590=CARTESIAN_POINT('Ctrl Pts',(25.0000000000001,1.38434137533096E-13,
179.500000000001));
#2591=CARTESIAN_POINT('Ctrl Pts',(25.0000000000001,0.49999999999947,179.500000000001));
#2592=CARTESIAN_POINT('Ctrl Pts',(25.,0.499999999999471,180.000000000001));
#2593=CARTESIAN_POINT('Ctrl Pts',(24.9999999999999,0.49999999999947,180.5));
#2594=CARTESIAN_POINT('Ctrl Pts',(24.9999999999999,1.38434137533096E-13,
180.5));
#2595=CARTESIAN_POINT('',(21.5,-3.99999999999999,180.));
#2596=CARTESIAN_POINT('',(21.5,1.81866079035945E-14,184.));
#2597=CARTESIAN_POINT('Origin',(21.5,0.,180.));
#2598=CARTESIAN_POINT('',(25.,-6.12323399573644E-17,180.5));
#2599=CARTESIAN_POINT('Origin',(21.5,1.86152342832779E-14,180.5));
#2600=CARTESIAN_POINT('Origin',(25.,0.,180.));
#2601=CARTESIAN_POINT('Origin',(21.5,0.,180.));
#2602=CARTESIAN_POINT('Origin',(0.,0.,180.));
#2603=CARTESIAN_POINT('',(15.,-3.99999999999999,180.));
#2604=CARTESIAN_POINT('',(0.,-3.99999999999999,180.));
#2605=CARTESIAN_POINT('Origin',(15.,0.,180.));
#2606=CARTESIAN_POINT('Origin',(25.,0.,180.));
#2607=CARTESIAN_POINT('Origin',(15.,0.,180.));
#2608=CARTESIAN_POINT('',(0.,0.,0.));
#2609=CARTESIAN_POINT('Origin',(-2.,0.,320.));
#2610=CARTESIAN_POINT('',(-21.6333076527839,3.99999999999999,320.));
#2611=CARTESIAN_POINT('',(-21.6333076527839,-3.99999999999999,320.));
#2612=CARTESIAN_POINT('Ctrl Pts',(-21.6333076527839,3.99999999999999,320.));
#2613=CARTESIAN_POINT('Ctrl Pts',(-21.6333076527839,3.99999999999999,320.503464233368));
#2614=CARTESIAN_POINT('Ctrl Pts',(-21.6527030440414,3.8991527689292,321.039701419423));
#2615=CARTESIAN_POINT('Ctrl Pts',(-21.7223085379416,3.49059487648095,322.024875180559));
#2616=CARTESIAN_POINT('Ctrl Pts',(-21.7714644430193,3.18294364927552,322.473910600217));
#2617=CARTESIAN_POINT('Ctrl Pts',(-21.8633822681921,2.47392407847503,323.182930171017));
#2618=CARTESIAN_POINT('Ctrl Pts',(-21.9121811723043,2.02488289993504,323.490591965245));
#2619=CARTESIAN_POINT('Ctrl Pts',(-21.9809663284242,1.03968925279594,323.899157524467));
#2620=CARTESIAN_POINT('Ctrl Pts',(-22.,0.503445092311466,324.));
#2621=CARTESIAN_POINT('Ctrl Pts',(-22.,-0.503445092311465,324.));
#2622=CARTESIAN_POINT('Ctrl Pts',(-21.9809663284242,-1.03968925279593,323.899157524467));
#2623=CARTESIAN_POINT('Ctrl Pts',(-21.9121811723043,-2.02488289993504,323.490591965245));
#2624=CARTESIAN_POINT('Ctrl Pts',(-21.8633822681921,-2.47392407847502,323.182930171017));
#2625=CARTESIAN_POINT('Ctrl Pts',(-21.7714644430193,-3.18294364927552,322.473910600217));
#2626=CARTESIAN_POINT('Ctrl Pts',(-21.7223085379416,-3.49059487648095,322.024875180559));
#2627=CARTESIAN_POINT('Ctrl Pts',(-21.6527030440414,-3.8991527689292,321.039701419423));
#2628=CARTESIAN_POINT('Ctrl Pts',(-21.6333076527839,-3.99999999999999,320.503464233368));
#2629=CARTESIAN_POINT('Ctrl Pts',(-21.6333076527839,-3.99999999999999,320.));
#2630=CARTESIAN_POINT('Ctrl Pts',(-21.6333076527839,-3.99999999999999,320.));
#2631=CARTESIAN_POINT('Ctrl Pts',(-21.6333076527839,-3.99999999999999,319.496535766632));
#2632=CARTESIAN_POINT('Ctrl Pts',(-21.6527030440414,-3.89915276892922,318.960298580577));
#2633=CARTESIAN_POINT('Ctrl Pts',(-21.7223085379416,-3.490594876481,317.975124819441));
#2634=CARTESIAN_POINT('Ctrl Pts',(-21.7714644430193,-3.18294364927552,317.526089399783));
#2635=CARTESIAN_POINT('Ctrl Pts',(-21.8633822681921,-2.47392407847502,316.817069828983));
#2636=CARTESIAN_POINT('Ctrl Pts',(-21.9121811723043,-2.02488289993508,316.509408034755));
#2637=CARTESIAN_POINT('Ctrl Pts',(-21.9809663284242,-1.039689252796,316.100842475533));
#2638=CARTESIAN_POINT('Ctrl Pts',(-22.,-0.503445092311466,316.));
#2639=CARTESIAN_POINT('Ctrl Pts',(-22.,0.503445092311465,316.));
#2640=CARTESIAN_POINT('Ctrl Pts',(-21.9809663284242,1.03968925279597,316.100842475533));
#2641=CARTESIAN_POINT('Ctrl Pts',(-21.9121811723043,2.02488289993506,316.509408034754));
#2642=CARTESIAN_POINT('Ctrl Pts',(-21.8633822681921,2.47392407847503,316.817069828983));
#2643=CARTESIAN_POINT('Ctrl Pts',(-21.7714644430193,3.18294364927552,317.526089399783));
#2644=CARTESIAN_POINT('Ctrl Pts',(-21.7223085379416,3.49059487648096,317.975124819441));
#2645=CARTESIAN_POINT('Ctrl Pts',(-21.6527030440414,3.8991527689292,318.960298580577));
#2646=CARTESIAN_POINT('Ctrl Pts',(-21.6333076527839,3.99999999999999,319.496535766632));
#2647=CARTESIAN_POINT('Ctrl Pts',(-21.6333076527839,3.99999999999999,320.));
#2648=CARTESIAN_POINT('',(-19.5959179422654,-3.99999999999999,320.));
#2649=CARTESIAN_POINT('',(-2.,-3.99999999999999,320.));
#2650=CARTESIAN_POINT('',(-19.5959179422654,3.99999999999999,320.));
#2651=CARTESIAN_POINT('Ctrl Pts',(-19.5959179422654,3.99999999999999,320.));
#2652=CARTESIAN_POINT('Ctrl Pts',(-19.5959179422654,3.99999999999999,319.496272992146));
#2653=CARTESIAN_POINT('Ctrl Pts',(-19.6173550647379,3.89905118499443,318.959928891352));
#2654=CARTESIAN_POINT('Ctrl Pts',(-19.6941660317108,3.4904216705935,317.97483197988));
#2655=CARTESIAN_POINT('Ctrl Pts',(-19.7483634040773,3.18281240876835,317.525958159276));
#2656=CARTESIAN_POINT('Ctrl Pts',(-19.8496135055327,2.47406169858037,316.817207449088));
#2657=CARTESIAN_POINT('Ctrl Pts',(-19.9033338860745,2.02517944479051,316.509582633821));
#2658=CARTESIAN_POINT('Ctrl Pts',(-19.9790475458833,1.04005322432747,316.100941831057));
#2659=CARTESIAN_POINT('Ctrl Pts',(-20.,0.503698781685597,316.));
#2660=CARTESIAN_POINT('Ctrl Pts',(-20.,-0.503698781685597,316.));
#2661=CARTESIAN_POINT('Ctrl Pts',(-19.9790475458833,-1.04005322432746,316.100941831057));
#2662=CARTESIAN_POINT('Ctrl Pts',(-19.9033338860745,-2.02517944479051,316.509582633821));
#2663=CARTESIAN_POINT('Ctrl Pts',(-19.8496135055327,-2.47406169858037,316.817207449088));
#2664=CARTESIAN_POINT('Ctrl Pts',(-19.7483634040773,-3.18281240876835,317.525958159276));
#2665=CARTESIAN_POINT('Ctrl Pts',(-19.6941660317108,-3.49042167059353,317.97483197988));
#2666=CARTESIAN_POINT('Ctrl Pts',(-19.6173550647379,-3.89905118499443,318.959928891352));
#2667=CARTESIAN_POINT('Ctrl Pts',(-19.5959179422654,-3.99999999999999,319.496272992146));
#2668=CARTESIAN_POINT('Ctrl Pts',(-19.5959179422654,-3.99999999999999,320.));
#2669=CARTESIAN_POINT('Ctrl Pts',(-19.5959179422654,-3.99999999999999,320.));
#2670=CARTESIAN_POINT('Ctrl Pts',(-19.5959179422654,-3.99999999999999,320.503727007854));
#2671=CARTESIAN_POINT('Ctrl Pts',(-19.6173550647379,-3.89905118499446,321.040071108647));
#2672=CARTESIAN_POINT('Ctrl Pts',(-19.6941660317108,-3.49042167059358,322.02516802012));
#2673=CARTESIAN_POINT('Ctrl Pts',(-19.7483634040773,-3.18281240876835,322.474041840724));
#2674=CARTESIAN_POINT('Ctrl Pts',(-19.8496135055327,-2.47406169858037,323.182792550912));
#2675=CARTESIAN_POINT('Ctrl Pts',(-19.9033338860745,-2.02517944479054,323.490417366179));
#2676=CARTESIAN_POINT('Ctrl Pts',(-19.9790475458833,-1.04005322432751,323.899058168943));
#2677=CARTESIAN_POINT('Ctrl Pts',(-20.,-0.503698781685598,324.));
#2678=CARTESIAN_POINT('Ctrl Pts',(-20.,0.503698781685596,324.));
#2679=CARTESIAN_POINT('Ctrl Pts',(-19.9790475458833,1.04005322432751,323.899058168943));
#2680=CARTESIAN_POINT('Ctrl Pts',(-19.9033338860745,2.02517944479053,323.490417366179));
#2681=CARTESIAN_POINT('Ctrl Pts',(-19.8496135055327,2.47406169858037,323.182792550912));
#2682=CARTESIAN_POINT('Ctrl Pts',(-19.7483634040773,3.18281240876835,322.474041840724));
#2683=CARTESIAN_POINT('Ctrl Pts',(-19.6941660317108,3.49042167059358,322.02516802012));
#2684=CARTESIAN_POINT('Ctrl Pts',(-19.6173550647379,3.89905118499446,321.040071108647));
#2685=CARTESIAN_POINT('Ctrl Pts',(-19.5959179422654,3.99999999999999,320.503727007854));
#2686=CARTESIAN_POINT('Ctrl Pts',(-19.5959179422654,3.99999999999999,320.));
#2687=CARTESIAN_POINT('Origin',(2.,0.,320.));
#2688=CARTESIAN_POINT('',(19.5959179422654,3.99999999999999,320.));
#2689=CARTESIAN_POINT('',(20.,1.08586892106921E-15,324.));
#2690=CARTESIAN_POINT('Ctrl Pts',(19.5959179422654,3.99999999999999,320.));
#2691=CARTESIAN_POINT('Ctrl Pts',(19.5959179422654,3.99999999999998,320.503727007854));
#2692=CARTESIAN_POINT('Ctrl Pts',(19.6173550647379,3.89905118499446,321.040071108647));
#2693=CARTESIAN_POINT('Ctrl Pts',(19.6941660317108,3.49042167059358,322.02516802012));
#2694=CARTESIAN_POINT('Ctrl Pts',(19.7483634040773,3.18281240876835,322.474041840724));
#2695=CARTESIAN_POINT('Ctrl Pts',(19.8496135055327,2.47406169858037,323.182792550912));
#2696=CARTESIAN_POINT('Ctrl Pts',(19.9033338860745,2.02517944479053,323.490417366179));
#2697=CARTESIAN_POINT('Ctrl Pts',(19.9790475458833,1.04005322432751,323.899058168943));
#2698=CARTESIAN_POINT('Ctrl Pts',(20.,0.503698781685599,324.));
#2699=CARTESIAN_POINT('Ctrl Pts',(20.,2.63677968348475E-15,324.));
#2700=CARTESIAN_POINT('',(20.,4.00020436071024E-15,316.));
#2701=CARTESIAN_POINT('Ctrl Pts',(20.,5.55111512312578E-15,316.));
#2702=CARTESIAN_POINT('Ctrl Pts',(20.,0.503698781685603,316.));
#2703=CARTESIAN_POINT('Ctrl Pts',(19.9790475458833,1.04005322432747,316.100941831057));
#2704=CARTESIAN_POINT('Ctrl Pts',(19.9033338860745,2.02517944479051,316.509582633821));
#2705=CARTESIAN_POINT('Ctrl Pts',(19.8496135055327,2.47406169858037,316.817207449088));
#2706=CARTESIAN_POINT('Ctrl Pts',(19.7483634040773,3.18281240876835,317.525958159276));
#2707=CARTESIAN_POINT('Ctrl Pts',(19.6941660317108,3.4904216705935,317.97483197988));
#2708=CARTESIAN_POINT('Ctrl Pts',(19.6173550647379,3.89905118499443,318.959928891352));
#2709=CARTESIAN_POINT('Ctrl Pts',(19.5959179422654,3.99999999999999,319.496272992146));
#2710=CARTESIAN_POINT('Ctrl Pts',(19.5959179422654,3.99999999999999,320.));
#2711=CARTESIAN_POINT('',(19.5959179422654,-3.99999999999999,320.));
#2712=CARTESIAN_POINT('Ctrl Pts',(19.5959179422654,-3.99999999999999,320.));
#2713=CARTESIAN_POINT('Ctrl Pts',(19.5959179422654,-3.99999999999999,319.496272992146));
#2714=CARTESIAN_POINT('Ctrl Pts',(19.6173550647379,-3.89905118499443,318.959928891352));
#2715=CARTESIAN_POINT('Ctrl Pts',(19.6941660317108,-3.49042167059353,317.97483197988));
#2716=CARTESIAN_POINT('Ctrl Pts',(19.7483634040773,-3.18281240876835,317.525958159276));
#2717=CARTESIAN_POINT('Ctrl Pts',(19.8496135055327,-2.47406169858037,316.817207449088));
#2718=CARTESIAN_POINT('Ctrl Pts',(19.9033338860745,-2.0251794447905,316.509582633821));
#2719=CARTESIAN_POINT('Ctrl Pts',(19.9790475458833,-1.04005322432746,316.100941831057));
#2720=CARTESIAN_POINT('Ctrl Pts',(20.,-0.503698781685596,316.));
#2721=CARTESIAN_POINT('Ctrl Pts',(20.,2.77555756156289E-16,316.));
#2722=CARTESIAN_POINT('',(21.6333076527839,-3.99999999999999,320.));
#2723=CARTESIAN_POINT('',(2.,-3.99999999999999,320.));
#2724=CARTESIAN_POINT('',(22.,2.59611238176539E-15,316.));
#2725=CARTESIAN_POINT('Ctrl Pts',(22.,2.77555756156289E-15,316.));
#2726=CARTESIAN_POINT('Ctrl Pts',(22.,-0.503445092311463,316.));
#2727=CARTESIAN_POINT('Ctrl Pts',(21.9809663284242,-1.03968925279597,316.100842475533));
#2728=CARTESIAN_POINT('Ctrl Pts',(21.9121811723043,-2.02488289993505,316.509408034754));
#2729=CARTESIAN_POINT('Ctrl Pts',(21.8633822681921,-2.47392407847502,316.817069828983));
#2730=CARTESIAN_POINT('Ctrl Pts',(21.7714644430193,-3.18294364927552,317.526089399783));
#2731=CARTESIAN_POINT('Ctrl Pts',(21.7223085379416,-3.49059487648096,317.975124819441));
#2732=CARTESIAN_POINT('Ctrl Pts',(21.6527030440414,-3.8991527689292,318.960298580577));
#2733=CARTESIAN_POINT('Ctrl Pts',(21.6333076527839,-3.99999999999999,319.496535766632));
#2734=CARTESIAN_POINT('Ctrl Pts',(21.6333076527839,-3.99999999999999,320.));
#2735=CARTESIAN_POINT('',(21.6333076527839,4.,320.));
#2736=CARTESIAN_POINT('Ctrl Pts',(21.6333076527839,4.,320.));
#2737=CARTESIAN_POINT('Ctrl Pts',(21.6333076527839,4.,319.496535766632));
#2738=CARTESIAN_POINT('Ctrl Pts',(21.6527030440414,3.8991527689292,318.960298580577));
#2739=CARTESIAN_POINT('Ctrl Pts',(21.7223085379416,3.49059487648096,317.975124819441));
#2740=CARTESIAN_POINT('Ctrl Pts',(21.7714644430193,3.18294364927552,317.526089399783));
#2741=CARTESIAN_POINT('Ctrl Pts',(21.8633822681921,2.47392407847503,316.817069828983));
#2742=CARTESIAN_POINT('Ctrl Pts',(21.9121811723043,2.02488289993506,316.509408034754));
#2743=CARTESIAN_POINT('Ctrl Pts',(21.9809663284242,1.03968925279597,316.100842475533));
#2744=CARTESIAN_POINT('Ctrl Pts',(22.,0.50344509231146,316.));
#2745=CARTESIAN_POINT('Ctrl Pts',(22.,-5.13478148889135E-15,316.));
#2746=CARTESIAN_POINT('',(22.,4.45055271554149E-16,324.));
#2747=CARTESIAN_POINT('Ctrl Pts',(22.,-1.2490009027033E-15,324.));
#2748=CARTESIAN_POINT('Ctrl Pts',(22.,0.503445092311465,324.));
#2749=CARTESIAN_POINT('Ctrl Pts',(21.9809663284242,1.03968925279594,323.899157524467));
#2750=CARTESIAN_POINT('Ctrl Pts',(21.9121811723043,2.02488289993504,323.490591965245));
#2751=CARTESIAN_POINT('Ctrl Pts',(21.8633822681921,2.47392407847503,323.182930171017));
#2752=CARTESIAN_POINT('Ctrl Pts',(21.7714644430193,3.18294364927552,322.473910600217));
#2753=CARTESIAN_POINT('Ctrl Pts',(21.7223085379416,3.49059487648095,322.024875180559));
#2754=CARTESIAN_POINT('Ctrl Pts',(21.6527030440414,3.8991527689292,321.039701419423));
#2755=CARTESIAN_POINT('Ctrl Pts',(21.6333076527839,3.99999999999999,320.503464233368));
#2756=CARTESIAN_POINT('Ctrl Pts',(21.6333076527839,3.99999999999999,320.));
#2757=CARTESIAN_POINT('Ctrl Pts',(21.6333076527839,-3.99999999999999,320.));
#2758=CARTESIAN_POINT('Ctrl Pts',(21.6333076527839,-3.99999999999999,320.503464233368));
#2759=CARTESIAN_POINT('Ctrl Pts',(21.6527030440414,-3.8991527689292,321.039701419423));
#2760=CARTESIAN_POINT('Ctrl Pts',(21.7223085379416,-3.49059487648095,322.024875180559));
#2761=CARTESIAN_POINT('Ctrl Pts',(21.7714644430193,-3.18294364927552,322.473910600217));
#2762=CARTESIAN_POINT('Ctrl Pts',(21.8633822681921,-2.47392407847502,323.182930171017));
#2763=CARTESIAN_POINT('Ctrl Pts',(21.9121811723043,-2.02488289993504,323.490591965245));
#2764=CARTESIAN_POINT('Ctrl Pts',(21.9809663284242,-1.03968925279594,323.899157524467));
#2765=CARTESIAN_POINT('Ctrl Pts',(22.,-0.503445092311467,324.));
#2766=CARTESIAN_POINT('Ctrl Pts',(22.,-1.38777878078145E-15,324.));
#2767=CARTESIAN_POINT('Ctrl Pts',(20.,-2.77555756156289E-16,324.));
#2768=CARTESIAN_POINT('Ctrl Pts',(20.,-0.503698781685597,324.));
#2769=CARTESIAN_POINT('Ctrl Pts',(19.9790475458833,-1.04005322432751,323.899058168943));
#2770=CARTESIAN_POINT('Ctrl Pts',(19.9033338860745,-2.02517944479053,323.490417366179));
#2771=CARTESIAN_POINT('Ctrl Pts',(19.8496135055327,-2.47406169858037,323.182792550912));
#2772=CARTESIAN_POINT('Ctrl Pts',(19.7483634040773,-3.18281240876835,322.474041840724));
#2773=CARTESIAN_POINT('Ctrl Pts',(19.6941660317108,-3.49042167059358,322.02516802012));
#2774=CARTESIAN_POINT('Ctrl Pts',(19.6173550647379,-3.89905118499446,321.040071108647));
#2775=CARTESIAN_POINT('Ctrl Pts',(19.5959179422654,-3.99999999999999,320.503727007854));
#2776=CARTESIAN_POINT('Ctrl Pts',(19.5959179422654,-3.99999999999999,320.));
#2777=CARTESIAN_POINT('Ctrl Pts',(-120.018678583471,4.99999999999999,180.));
#2778=CARTESIAN_POINT('Ctrl Pts',(168.003735716694,4.99999999999999,180.));
#2779=CARTESIAN_POINT('Ctrl Pts',(-120.018678583471,4.99999999999999,180.701429560647));
#2780=CARTESIAN_POINT('Ctrl Pts',(168.003735716694,4.99999999999999,180.701429560647));
#2781=CARTESIAN_POINT('Ctrl Pts',(-120.018678583471,4.84154118145123,181.452551073965));
#2782=CARTESIAN_POINT('Ctrl Pts',(168.003735716694,4.84154118145123,181.452551073965));
#2783=CARTESIAN_POINT('Ctrl Pts',(-120.018678583471,4.52635286465426,182.124177427767));
#2784=CARTESIAN_POINT('Ctrl Pts',(168.003735716694,4.52635286465426,182.124177427767));
#2785=CARTESIAN_POINT('Ctrl Pts',(-120.018678583471,4.03825843713571,183.164244788121));
#2786=CARTESIAN_POINT('Ctrl Pts',(168.003735716694,4.03825843713571,183.164244788121));
#2787=CARTESIAN_POINT('Ctrl Pts',(-120.018678583471,3.23871549390966,183.978582045816));
#2788=CARTESIAN_POINT('Ctrl Pts',(168.003735716694,3.23871549390966,183.978582045816));
#2789=CARTESIAN_POINT('Ctrl Pts',(-120.018678583471,2.20859185585293,184.485768832013));
#2790=CARTESIAN_POINT('Ctrl Pts',(168.003735716694,2.20859185585293,184.485768832013));
#2791=CARTESIAN_POINT('Ctrl Pts',(-120.018678583471,1.4855680314837,184.841753411221));
#2792=CARTESIAN_POINT('Ctrl Pts',(168.003735716694,1.4855680314837,184.841753411221));
#2793=CARTESIAN_POINT('Ctrl Pts',(-120.018678583471,0.672332306955193,185.013639583555));
#2794=CARTESIAN_POINT('Ctrl Pts',(168.003735716694,0.672332306955193,185.013639583555));
#2795=CARTESIAN_POINT('Ctrl Pts',(-120.018678583471,-0.0947408793825885,
184.999102335997));
#2796=CARTESIAN_POINT('Ctrl Pts',(168.003735716694,-0.0947408793825885,
184.999102335997));
#2797=CARTESIAN_POINT('Ctrl Pts',(-120.018678583471,-0.861749446049807,
184.984566313084));
#2798=CARTESIAN_POINT('Ctrl Pts',(168.003735716694,-0.861749446049807,184.984566313084));
#2799=CARTESIAN_POINT('Ctrl Pts',(-120.018678583471,-1.67892656531164,184.777834904611));
#2800=CARTESIAN_POINT('Ctrl Pts',(168.003735716694,-1.67892656531164,184.777834904611));
#2801=CARTESIAN_POINT('Ctrl Pts',(-120.018678583471,-2.38556209111995,184.394211363762));
#2802=CARTESIAN_POINT('Ctrl Pts',(168.003735716694,-2.38556209111995,184.394211363762));
#2803=CARTESIAN_POINT('Ctrl Pts',(-120.018678583471,-3.01025748817222,184.055072088397));
#2804=CARTESIAN_POINT('Ctrl Pts',(168.003735716694,-3.01025748817222,184.055072088397));
#2805=CARTESIAN_POINT('Ctrl Pts',(-120.018678583471,-3.52924546522797,183.609386777));
#2806=CARTESIAN_POINT('Ctrl Pts',(168.003735716694,-3.52924546522797,183.609386777));
#2807=CARTESIAN_POINT('Ctrl Pts',(-120.018678583471,-3.95462292501808,183.059568191906));
#2808=CARTESIAN_POINT('Ctrl Pts',(168.003735716694,-3.95462292501808,183.059568191906));
#2809=CARTESIAN_POINT('Ctrl Pts',(-120.018678583471,-4.56739501624512,182.267534019833));
#2810=CARTESIAN_POINT('Ctrl Pts',(168.003735716694,-4.56739501624512,182.267534019833));
#2811=CARTESIAN_POINT('Ctrl Pts',(-120.018678583471,-4.9464904141789,181.226327567706));
#2812=CARTESIAN_POINT('Ctrl Pts',(168.003735716694,-4.9464904141789,181.226327567706));
#2813=CARTESIAN_POINT('Ctrl Pts',(-120.018678583471,-4.99415183469097,180.241759078532));
#2814=CARTESIAN_POINT('Ctrl Pts',(168.003735716694,-4.99415183469097,180.241759078532));
#2815=CARTESIAN_POINT('Ctrl Pts',(-120.018678583471,-5.03115008136056,179.477465705943));
#2816=CARTESIAN_POINT('Ctrl Pts',(168.003735716694,-5.03115008136056,179.477465705943));
#2817=CARTESIAN_POINT('Ctrl Pts',(-120.018678583471,-4.88912990582069,178.683801029721));
#2818=CARTESIAN_POINT('Ctrl Pts',(168.003735716694,-4.88912990582069,178.683801029721));
#2819=CARTESIAN_POINT('Ctrl Pts',(-120.018678583471,-4.56312148257041,177.956003342639));
#2820=CARTESIAN_POINT('Ctrl Pts',(168.003735716694,-4.56312148257041,177.956003342639));
#2821=CARTESIAN_POINT('Ctrl Pts',(-120.018678583471,-4.07307618333385,176.862001439883));
#2822=CARTESIAN_POINT('Ctrl Pts',(168.003735716694,-4.07307618333385,176.862001439883));
#2823=CARTESIAN_POINT('Ctrl Pts',(-120.018678583471,-3.23595384820037,176.004517412987));
#2824=CARTESIAN_POINT('Ctrl Pts',(168.003735716694,-3.23595384820037,176.004517412987));
#2825=CARTESIAN_POINT('Ctrl Pts',(-120.018678583471,-2.15489635508168,175.488190861876));
#2826=CARTESIAN_POINT('Ctrl Pts',(168.003735716694,-2.15489635508168,175.488190861876));
#2827=CARTESIAN_POINT('Ctrl Pts',(-120.018678583471,-1.44740407601968,175.15028371937));
#2828=CARTESIAN_POINT('Ctrl Pts',(168.003735716694,-1.44740407601968,175.15028371937));
#2829=CARTESIAN_POINT('Ctrl Pts',(-120.018678583471,-0.657548063760293,
174.987640434044));
#2830=CARTESIAN_POINT('Ctrl Pts',(168.003735716694,-0.657548063760293,174.987640434044));
#2831=CARTESIAN_POINT('Ctrl Pts',(-120.018678583471,0.0880693581523543,
175.000775681353));
#2832=CARTESIAN_POINT('Ctrl Pts',(168.003735716694,0.0880693581523543,175.000775681353));
#2833=CARTESIAN_POINT('Ctrl Pts',(-120.018678583471,0.849005936014474,175.014180800174));
#2834=CARTESIAN_POINT('Ctrl Pts',(168.003735716694,0.849005936014474,175.014180800174));
#2835=CARTESIAN_POINT('Ctrl Pts',(-120.018678583471,1.65998081975207,175.216515933084));
#2836=CARTESIAN_POINT('Ctrl Pts',(168.003735716694,1.65998081975207,175.216515933084));
#2837=CARTESIAN_POINT('Ctrl Pts',(-120.018678583471,2.36345091283147,175.593856586238));
#2838=CARTESIAN_POINT('Ctrl Pts',(168.003735716694,2.36345091283147,175.593856586238));
#2839=CARTESIAN_POINT('Ctrl Pts',(-120.018678583471,3.04069695749377,175.957130686094));
#2840=CARTESIAN_POINT('Ctrl Pts',(168.003735716694,3.04069695749377,175.957130686094));
#2841=CARTESIAN_POINT('Ctrl Pts',(-120.018678583471,3.59636505476289,176.445115525822));
#2842=CARTESIAN_POINT('Ctrl Pts',(168.003735716694,3.59636505476289,176.445115525822));
#2843=CARTESIAN_POINT('Ctrl Pts',(-120.018678583471,4.041321668556,177.055900957634));
#2844=CARTESIAN_POINT('Ctrl Pts',(168.003735716694,4.041321668556,177.055900957634));
#2845=CARTESIAN_POINT('Ctrl Pts',(-120.018678583471,4.65481124319825,177.898029118324));
#2846=CARTESIAN_POINT('Ctrl Pts',(168.003735716694,4.65481124319825,177.898029118324));
#2847=CARTESIAN_POINT('Ctrl Pts',(-120.018678583471,4.99999999999999,178.995710165759));
#2848=CARTESIAN_POINT('Ctrl Pts',(168.003735716694,4.99999999999999,178.995710165759));
#2849=CARTESIAN_POINT('Ctrl Pts',(-120.018678583471,4.99999999999999,180.));
#2850=CARTESIAN_POINT('Ctrl Pts',(168.003735716694,4.99999999999999,180.));
#2851=CARTESIAN_POINT('',(-19.3649167310371,4.99999999999999,180.));
#2852=CARTESIAN_POINT('Ctrl Pts',(-19.3649167310371,4.99999999999999,180.));
#2853=CARTESIAN_POINT('Ctrl Pts',(-19.3649167310371,4.99999999999999,179.656276636379));
#2854=CARTESIAN_POINT('Ctrl Pts',(-19.3752683254359,4.96098012900332,179.265182649221));
#2855=CARTESIAN_POINT('Ctrl Pts',(-19.4353496242784,4.72078509063997,178.290368141715));
#2856=CARTESIAN_POINT('Ctrl Pts',(-19.4914325180833,4.50873512303266,177.690061693343));
#2857=CARTESIAN_POINT('Ctrl Pts',(-19.6698374497908,3.64021897653246,176.511459386496));
#2858=CARTESIAN_POINT('Ctrl Pts',(-19.7561738615341,3.167765149487,176.070768115353));
#2859=CARTESIAN_POINT('Ctrl Pts',(-19.9267480044898,1.86096567166663,175.283608655792));
#2860=CARTESIAN_POINT('Ctrl Pts',(-19.9693191762704,1.18642139031165,175.126999474205));
#2861=CARTESIAN_POINT('Ctrl Pts',(-19.9994091583083,0.396121730007714,175.002722388395));
#2862=CARTESIAN_POINT('Ctrl Pts',(-20.0166801524078,-0.277043159907006,
174.932154696418));
#2863=CARTESIAN_POINT('Ctrl Pts',(-19.9244729893901,-1.8944504241017,175.309555396068));
#2864=CARTESIAN_POINT('Ctrl Pts',(-19.8487454717896,-2.4936420409959,175.633241025647));
#2865=CARTESIAN_POINT('Ctrl Pts',(-19.7469625775935,-3.18189012768007,176.126727194768));
#2866=CARTESIAN_POINT('Ctrl Pts',(-19.7059339958017,-3.4246715612765,176.337559801306));
#2867=CARTESIAN_POINT('Ctrl Pts',(-19.5708409016226,-4.15261418047417,177.114358081489));
#2868=CARTESIAN_POINT('Ctrl Pts',(-19.4964574660857,-4.46350630203481,177.693390357527));
#2869=CARTESIAN_POINT('Ctrl Pts',(-19.3986283838268,-4.87322999505193,178.723777174646));
#2870=CARTESIAN_POINT('Ctrl Pts',(-19.3650256499815,-4.99957814958542,179.355073383189));
#2871=CARTESIAN_POINT('Ctrl Pts',(-19.3649475283197,-4.99988072118004,180.002013330726));
#2872=CARTESIAN_POINT('Ctrl Pts',(-19.3649106763447,-5.00002345189721,180.307191359079));
#2873=CARTESIAN_POINT('Ctrl Pts',(-19.3736373833142,-4.97254785920772,180.890223123103));
#2874=CARTESIAN_POINT('Ctrl Pts',(-19.4674269397344,-4.58693311377117,182.017619598821));
#2875=CARTESIAN_POINT('Ctrl Pts',(-19.5183192231322,-4.38551433152747,182.504339680886));
#2876=CARTESIAN_POINT('Ctrl Pts',(-19.6865149822651,-3.55062826109306,183.580157065446));
#2877=CARTESIAN_POINT('Ctrl Pts',(-19.7728418386983,-3.06434838205126,184.009862697332));
#2878=CARTESIAN_POINT('Ctrl Pts',(-19.939001955482,-1.73069169664475,184.767170010893));
#2879=CARTESIAN_POINT('Ctrl Pts',(-19.9761019161117,-1.06408188475894,184.900835849746));
#2880=CARTESIAN_POINT('Ctrl Pts',(-20.0120505317368,0.05230497848514,185.049843619988));
#2881=CARTESIAN_POINT('Ctrl Pts',(-19.9957915020587,0.694184741132029,184.982611117669));
#2882=CARTESIAN_POINT('Ctrl Pts',(-19.9134632202362,2.00564095945725,184.644423471671));
#2883=CARTESIAN_POINT('Ctrl Pts',(-19.8352703571503,2.5969441803465,184.305982645319));
#2884=CARTESIAN_POINT('Ctrl Pts',(-19.6928469146564,3.52972547721907,183.604186924279));
#2885=CARTESIAN_POINT('Ctrl Pts',(-19.6057167803969,3.96687494742429,183.120476018664));
#2886=CARTESIAN_POINT('Ctrl Pts',(-19.4373578240358,4.73060594531999,181.819624478891));
#2887=CARTESIAN_POINT('Ctrl Pts',(-19.3940863845552,4.88606300001282,181.13758993203));
#2888=CARTESIAN_POINT('Ctrl Pts',(-19.3704556074501,4.97859341571146,180.495886648245));
#2889=CARTESIAN_POINT('Ctrl Pts',(-19.3649167310371,4.99999999999999,180.261670622645));
#2890=CARTESIAN_POINT('Ctrl Pts',(-19.3649167310371,4.99999999999999,180.));
#2891=CARTESIAN_POINT('',(-21.4242852856286,4.99999999999999,180.));
#2892=CARTESIAN_POINT('',(-120.018678583471,4.99999999999999,180.));
#2893=CARTESIAN_POINT('Ctrl Pts',(-21.4242852856285,4.99999999999999,180.));
#2894=CARTESIAN_POINT('Ctrl Pts',(-21.4242852856285,4.99999999999999,180.266440972911));
#2895=CARTESIAN_POINT('Ctrl Pts',(-21.4295159134836,4.97766066683645,180.513637485348));
#2896=CARTESIAN_POINT('Ctrl Pts',(-21.4572794964352,4.85725414305748,181.305693804631));
#2897=CARTESIAN_POINT('Ctrl Pts',(-21.5035090198973,4.66401988009852,181.947578824682));
#2898=CARTESIAN_POINT('Ctrl Pts',(-21.6463171087964,3.94382916021953,183.146091812383));
#2899=CARTESIAN_POINT('Ctrl Pts',(-21.7252323873223,3.5068141199092,183.629254356169));
#2900=CARTESIAN_POINT('Ctrl Pts',(-21.8542780588982,2.56268308232979,184.325029328962));
#2901=CARTESIAN_POINT('Ctrl Pts',(-21.9246427130955,1.97682230622835,184.659570461731));
#2902=CARTESIAN_POINT('Ctrl Pts',(-21.9975587820033,0.647370837356641,184.988682812051));
#2903=CARTESIAN_POINT('Ctrl Pts',(-22.0114635671403,0.00763006450754167,
185.052019663629));
#2904=CARTESIAN_POINT('Ctrl Pts',(-21.9724550534794,-1.21362618186779,184.874411158033));
#2905=CARTESIAN_POINT('Ctrl Pts',(-21.932682388788,-1.8531096149277,184.710535799577));
#2906=CARTESIAN_POINT('Ctrl Pts',(-21.7670508838473,-3.27877993846323,183.872852240133));
#2907=CARTESIAN_POINT('Ctrl Pts',(-21.6835800732439,-3.72748016875351,183.362046973031));
#2908=CARTESIAN_POINT('Ctrl Pts',(-21.575660584424,-4.31251978640233,182.58467155384));
#2909=CARTESIAN_POINT('Ctrl Pts',(-21.5217853693328,-4.56550119232117,182.090718612903));
#2910=CARTESIAN_POINT('Ctrl Pts',(-21.4320915723086,-4.9722430980436,180.876072778015));
#2911=CARTESIAN_POINT('Ctrl Pts',(-21.4242940461624,-4.99996246291467,180.30793729798));
#2912=CARTESIAN_POINT('Ctrl Pts',(-21.4243130374363,-4.99988108597961,180.003006565595));
#2913=CARTESIAN_POINT('Ctrl Pts',(-21.4243525248944,-4.99971188362311,179.368981722491));
#2914=CARTESIAN_POINT('Ctrl Pts',(-21.4537490423155,-4.87805507940704,178.732432901037));
#2915=CARTESIAN_POINT('Ctrl Pts',(-21.534494160282,-4.50391537304462,177.797069546953));
#2916=CARTESIAN_POINT('Ctrl Pts',(-21.5996533102872,-4.21889499554481,177.181822069633));
#2917=CARTESIAN_POINT('Ctrl Pts',(-21.7335221221638,-3.42103550068265,176.334952896946));
#2918=CARTESIAN_POINT('Ctrl Pts',(-21.7707205591023,-3.17898668973262,176.123720780895));
#2919=CARTESIAN_POINT('Ctrl Pts',(-21.8626420423699,-2.49167222733435,175.63336844862));
#2920=CARTESIAN_POINT('Ctrl Pts',(-21.9314709722171,-1.89940358158573,175.308986444414));
#2921=CARTESIAN_POINT('Ctrl Pts',(-22.0142761168708,-0.286050077143755,
174.936162313307));
#2922=CARTESIAN_POINT('Ctrl Pts',(-21.9996100525413,0.401172811047044,175.002073703072));
#2923=CARTESIAN_POINT('Ctrl Pts',(-21.9678642907813,1.29586484146865,175.14626218032));
#2924=CARTESIAN_POINT('Ctrl Pts',(-21.9249239566795,1.93920230775896,175.325326856333));
#2925=CARTESIAN_POINT('Ctrl Pts',(-21.7768529503723,3.17624999439771,176.0805697055));
#2926=CARTESIAN_POINT('Ctrl Pts',(-21.6987511052204,3.64994229125153,176.518949199742));
#2927=CARTESIAN_POINT('Ctrl Pts',(-21.5378339057897,4.51120696935556,177.700558030938));
#2928=CARTESIAN_POINT('Ctrl Pts',(-21.4865439748271,4.72726309970277,178.303589812472));
#2929=CARTESIAN_POINT('Ctrl Pts',(-21.433923111627,4.95956788576955,179.269828034558));
#2930=CARTESIAN_POINT('Ctrl Pts',(-21.4242852856285,4.99999999999999,179.651385925244));
#2931=CARTESIAN_POINT('Ctrl Pts',(-21.4242852856285,4.99999999999999,180.));
#2932=CARTESIAN_POINT('Ctrl Pts',(-120.018678583471,4.99999999999999,180.));
#2933=CARTESIAN_POINT('Ctrl Pts',(168.003735716694,4.99999999999999,180.));
#2934=CARTESIAN_POINT('Ctrl Pts',(-120.018678583471,4.99999999999999,180.701429560647));
#2935=CARTESIAN_POINT('Ctrl Pts',(168.003735716694,4.99999999999999,180.701429560647));
#2936=CARTESIAN_POINT('Ctrl Pts',(-120.018678583471,4.84154118145123,181.452551073965));
#2937=CARTESIAN_POINT('Ctrl Pts',(168.003735716694,4.84154118145123,181.452551073965));
#2938=CARTESIAN_POINT('Ctrl Pts',(-120.018678583471,4.52635286465426,182.124177427767));
#2939=CARTESIAN_POINT('Ctrl Pts',(168.003735716694,4.52635286465426,182.124177427767));
#2940=CARTESIAN_POINT('Ctrl Pts',(-120.018678583471,4.03825843713571,183.164244788121));
#2941=CARTESIAN_POINT('Ctrl Pts',(168.003735716694,4.03825843713571,183.164244788121));
#2942=CARTESIAN_POINT('Ctrl Pts',(-120.018678583471,3.23871549390966,183.978582045816));
#2943=CARTESIAN_POINT('Ctrl Pts',(168.003735716694,3.23871549390966,183.978582045816));
#2944=CARTESIAN_POINT('Ctrl Pts',(-120.018678583471,2.20859185585293,184.485768832013));
#2945=CARTESIAN_POINT('Ctrl Pts',(168.003735716694,2.20859185585293,184.485768832013));
#2946=CARTESIAN_POINT('Ctrl Pts',(-120.018678583471,1.4855680314837,184.841753411221));
#2947=CARTESIAN_POINT('Ctrl Pts',(168.003735716694,1.4855680314837,184.841753411221));
#2948=CARTESIAN_POINT('Ctrl Pts',(-120.018678583471,0.672332306955193,185.013639583555));
#2949=CARTESIAN_POINT('Ctrl Pts',(168.003735716694,0.672332306955193,185.013639583555));
#2950=CARTESIAN_POINT('Ctrl Pts',(-120.018678583471,-0.0947408793825885,
184.999102335997));
#2951=CARTESIAN_POINT('Ctrl Pts',(168.003735716694,-0.0947408793825885,
184.999102335997));
#2952=CARTESIAN_POINT('Ctrl Pts',(-120.018678583471,-0.861749446049807,
184.984566313084));
#2953=CARTESIAN_POINT('Ctrl Pts',(168.003735716694,-0.861749446049807,184.984566313084));
#2954=CARTESIAN_POINT('Ctrl Pts',(-120.018678583471,-1.67892656531164,184.777834904611));
#2955=CARTESIAN_POINT('Ctrl Pts',(168.003735716694,-1.67892656531164,184.777834904611));
#2956=CARTESIAN_POINT('Ctrl Pts',(-120.018678583471,-2.38556209111995,184.394211363762));
#2957=CARTESIAN_POINT('Ctrl Pts',(168.003735716694,-2.38556209111995,184.394211363762));
#2958=CARTESIAN_POINT('Ctrl Pts',(-120.018678583471,-3.01025748817222,184.055072088397));
#2959=CARTESIAN_POINT('Ctrl Pts',(168.003735716694,-3.01025748817222,184.055072088397));
#2960=CARTESIAN_POINT('Ctrl Pts',(-120.018678583471,-3.52924546522797,183.609386777));
#2961=CARTESIAN_POINT('Ctrl Pts',(168.003735716694,-3.52924546522797,183.609386777));
#2962=CARTESIAN_POINT('Ctrl Pts',(-120.018678583471,-3.95462292501808,183.059568191906));
#2963=CARTESIAN_POINT('Ctrl Pts',(168.003735716694,-3.95462292501808,183.059568191906));
#2964=CARTESIAN_POINT('Ctrl Pts',(-120.018678583471,-4.56739501624512,182.267534019833));
#2965=CARTESIAN_POINT('Ctrl Pts',(168.003735716694,-4.56739501624512,182.267534019833));
#2966=CARTESIAN_POINT('Ctrl Pts',(-120.018678583471,-4.9464904141789,181.226327567706));
#2967=CARTESIAN_POINT('Ctrl Pts',(168.003735716694,-4.9464904141789,181.226327567706));
#2968=CARTESIAN_POINT('Ctrl Pts',(-120.018678583471,-4.99415183469097,180.241759078532));
#2969=CARTESIAN_POINT('Ctrl Pts',(168.003735716694,-4.99415183469097,180.241759078532));
#2970=CARTESIAN_POINT('Ctrl Pts',(-120.018678583471,-5.03115008136056,179.477465705943));
#2971=CARTESIAN_POINT('Ctrl Pts',(168.003735716694,-5.03115008136056,179.477465705943));
#2972=CARTESIAN_POINT('Ctrl Pts',(-120.018678583471,-4.88912990582069,178.683801029721));
#2973=CARTESIAN_POINT('Ctrl Pts',(168.003735716694,-4.88912990582069,178.683801029721));
#2974=CARTESIAN_POINT('Ctrl Pts',(-120.018678583471,-4.56312148257041,177.956003342639));
#2975=CARTESIAN_POINT('Ctrl Pts',(168.003735716694,-4.56312148257041,177.956003342639));
#2976=CARTESIAN_POINT('Ctrl Pts',(-120.018678583471,-4.07307618333385,176.862001439883));
#2977=CARTESIAN_POINT('Ctrl Pts',(168.003735716694,-4.07307618333385,176.862001439883));
#2978=CARTESIAN_POINT('Ctrl Pts',(-120.018678583471,-3.23595384820037,176.004517412987));
#2979=CARTESIAN_POINT('Ctrl Pts',(168.003735716694,-3.23595384820037,176.004517412987));
#2980=CARTESIAN_POINT('Ctrl Pts',(-120.018678583471,-2.15489635508168,175.488190861876));
#2981=CARTESIAN_POINT('Ctrl Pts',(168.003735716694,-2.15489635508168,175.488190861876));
#2982=CARTESIAN_POINT('Ctrl Pts',(-120.018678583471,-1.44740407601968,175.15028371937));
#2983=CARTESIAN_POINT('Ctrl Pts',(168.003735716694,-1.44740407601968,175.15028371937));
#2984=CARTESIAN_POINT('Ctrl Pts',(-120.018678583471,-0.657548063760293,
174.987640434044));
#2985=CARTESIAN_POINT('Ctrl Pts',(168.003735716694,-0.657548063760293,174.987640434044));
#2986=CARTESIAN_POINT('Ctrl Pts',(-120.018678583471,0.0880693581523543,
175.000775681353));
#2987=CARTESIAN_POINT('Ctrl Pts',(168.003735716694,0.0880693581523543,175.000775681353));
#2988=CARTESIAN_POINT('Ctrl Pts',(-120.018678583471,0.849005936014474,175.014180800174));
#2989=CARTESIAN_POINT('Ctrl Pts',(168.003735716694,0.849005936014474,175.014180800174));
#2990=CARTESIAN_POINT('Ctrl Pts',(-120.018678583471,1.65998081975207,175.216515933084));
#2991=CARTESIAN_POINT('Ctrl Pts',(168.003735716694,1.65998081975207,175.216515933084));
#2992=CARTESIAN_POINT('Ctrl Pts',(-120.018678583471,2.36345091283147,175.593856586238));
#2993=CARTESIAN_POINT('Ctrl Pts',(168.003735716694,2.36345091283147,175.593856586238));
#2994=CARTESIAN_POINT('Ctrl Pts',(-120.018678583471,3.04069695749377,175.957130686094));
#2995=CARTESIAN_POINT('Ctrl Pts',(168.003735716694,3.04069695749377,175.957130686094));
#2996=CARTESIAN_POINT('Ctrl Pts',(-120.018678583471,3.59636505476289,176.445115525822));
#2997=CARTESIAN_POINT('Ctrl Pts',(168.003735716694,3.59636505476289,176.445115525822));
#2998=CARTESIAN_POINT('Ctrl Pts',(-120.018678583471,4.041321668556,177.055900957634));
#2999=CARTESIAN_POINT('Ctrl Pts',(168.003735716694,4.041321668556,177.055900957634));
#3000=CARTESIAN_POINT('Ctrl Pts',(-120.018678583471,4.65481124319825,177.898029118324));
#3001=CARTESIAN_POINT('Ctrl Pts',(168.003735716694,4.65481124319825,177.898029118324));
#3002=CARTESIAN_POINT('Ctrl Pts',(-120.018678583471,4.99999999999999,178.995710165759));
#3003=CARTESIAN_POINT('Ctrl Pts',(168.003735716694,4.99999999999999,178.995710165759));
#3004=CARTESIAN_POINT('Ctrl Pts',(-120.018678583471,4.99999999999999,180.));
#3005=CARTESIAN_POINT('Ctrl Pts',(168.003735716694,4.99999999999999,180.));
#3006=CARTESIAN_POINT('',(19.3649167310371,4.99999999999999,180.));
#3007=CARTESIAN_POINT('',(20.,1.09783585004622E-9,184.999950279416));
#3008=CARTESIAN_POINT('Ctrl Pts',(19.3649167310371,4.99999999999999,180.000000000155));
#3009=CARTESIAN_POINT('Ctrl Pts',(19.3649167310393,4.9999999999915,180.255797976078));
#3010=CARTESIAN_POINT('Ctrl Pts',(19.3709161789166,4.98152900200967,180.815194883544));
#3011=CARTESIAN_POINT('Ctrl Pts',(19.4665112788902,4.5921654017984,182.065094951232));
#3012=CARTESIAN_POINT('Ctrl Pts',(19.5252939307559,4.33900973909425,182.52327366873));
#3013=CARTESIAN_POINT('Ctrl Pts',(19.6155368981629,3.90717831536256,183.14107477953));
#3014=CARTESIAN_POINT('Ctrl Pts',(19.6564128349259,3.69873883889033,183.384935096394));
#3015=CARTESIAN_POINT('Ctrl Pts',(19.7803706292242,2.99455052170116,184.060876404812));
#3016=CARTESIAN_POINT('Ctrl Pts',(19.8559843598647,2.45672095108571,184.394978623011));
#3017=CARTESIAN_POINT('Ctrl Pts',(19.9634978707024,1.33933912050469,184.855602695573));
#3018=CARTESIAN_POINT('Ctrl Pts',(19.9971565484544,0.709366488718439,184.987413058734));
#3019=CARTESIAN_POINT('Ctrl Pts',(19.9999400795374,0.0566981305842219,184.999642855756));
#3020=CARTESIAN_POINT('Ctrl Pts',(19.9999999999969,0.0282649299869405,184.999921943856));
#3021=CARTESIAN_POINT('Ctrl Pts',(20.,2.19566810046035E-9,184.999950279416));
#3022=CARTESIAN_POINT('',(21.4242852856286,4.99999999999999,180.));
#3023=CARTESIAN_POINT('',(-120.018678583471,4.99999999999999,180.));
#3024=CARTESIAN_POINT('',(22.,-1.18558479586405E-15,184.999950279418));
#3025=CARTESIAN_POINT('Ctrl Pts',(21.4242852856286,4.99999999999999,180.));
#3026=CARTESIAN_POINT('Ctrl Pts',(21.4242852856286,5.,180.331321770038));
#3027=CARTESIAN_POINT('Ctrl Pts',(21.4325987305796,4.96571390954325,180.744228596537));
#3028=CARTESIAN_POINT('Ctrl Pts',(21.5061118431463,4.64030421838038,182.04689533232));
#3029=CARTESIAN_POINT('Ctrl Pts',(21.5836207752017,4.26781713536477,182.642067445167));
#3030=CARTESIAN_POINT('Ctrl Pts',(21.7015310022096,3.63232448614424,183.501121906396));
#3031=CARTESIAN_POINT('Ctrl Pts',(21.7809360387086,3.15065181168726,183.942868874243));
#3032=CARTESIAN_POINT('Ctrl Pts',(21.9331646274147,1.85908336411556,184.714255119539));
#3033=CARTESIAN_POINT('Ctrl Pts',(21.9728125131015,1.18137916674032,184.876892121407));
#3034=CARTESIAN_POINT('Ctrl Pts',(21.9944951369469,0.532075416791465,184.974489363689));
#3035=CARTESIAN_POINT('Ctrl Pts',(22.,0.285584181637826,184.999663981717));
#3036=CARTESIAN_POINT('Ctrl Pts',(22.,-1.38777878078145E-15,184.999950279418));
#3037=CARTESIAN_POINT('',(22.,-4.42951769594068E-15,175.000041436246));
#3038=CARTESIAN_POINT('Ctrl Pts',(22.,-3.46944695195361E-17,184.999950279418));
#3039=CARTESIAN_POINT('Ctrl Pts',(22.,-0.343144993886238,185.000294281744));
#3040=CARTESIAN_POINT('Ctrl Pts',(21.9920148363644,-0.742730533301487,184.963404127961));
#3041=CARTESIAN_POINT('Ctrl Pts',(21.9288144272746,-1.90972866300947,184.67667933317));
#3042=CARTESIAN_POINT('Ctrl Pts',(21.861683715817,-2.50617516724031,184.363949860461));
#3043=CARTESIAN_POINT('Ctrl Pts',(21.7448558897055,-3.36520718643722,183.733751683529));
#3044=CARTESIAN_POINT('Ctrl Pts',(21.6678314528203,-3.82957681260466,183.304010209844));
#3045=CARTESIAN_POINT('Ctrl Pts',(21.5909137408081,-4.22284783493632,182.673663309574));
#3046=CARTESIAN_POINT('Ctrl Pts',(21.5494225341618,-4.43498739068646,182.333639499534));
#3047=CARTESIAN_POINT('Ctrl Pts',(21.5124934142766,-4.6075844188304,181.963622213912));
#3048=CARTESIAN_POINT('Ctrl Pts',(21.4569989662757,-4.85934461009825,181.214573663743));
#3049=CARTESIAN_POINT('Ctrl Pts',(21.4365908976517,-4.94710817987512,180.820242962523));
#3050=CARTESIAN_POINT('Ctrl Pts',(21.4166549039084,-5.03285024108842,179.835986416571));
#3051=CARTESIAN_POINT('Ctrl Pts',(21.4300169404193,-4.97942996428264,179.193141115726));
#3052=CARTESIAN_POINT('Ctrl Pts',(21.5179664983127,-4.58460297805858,177.889624577146));
#3053=CARTESIAN_POINT('Ctrl Pts',(21.5872551760404,-4.25995320613274,177.307263465564));
#3054=CARTESIAN_POINT('Ctrl Pts',(21.7294201940974,-3.46441716524137,176.332638954624));
#3055=CARTESIAN_POINT('Ctrl Pts',(21.8081204309277,-2.95990282534955,175.913024012782));
#3056=CARTESIAN_POINT('Ctrl Pts',(21.9452433538611,-1.69304720595882,175.234639236131));
#3057=CARTESIAN_POINT('Ctrl Pts',(21.9816800346771,-1.04378161264859,175.083306187542));
#3058=CARTESIAN_POINT('Ctrl Pts',(21.9981718056279,-0.334310676329425,175.008708067723));
#3059=CARTESIAN_POINT('Ctrl Pts',(22.,-0.163664525260938,175.000188837908));
#3060=CARTESIAN_POINT('Ctrl Pts',(22.,-8.95117313604032E-15,175.000041436246));
#3061=CARTESIAN_POINT('Ctrl Pts',(22.,-8.07513778067204E-15,175.000041436246));
#3062=CARTESIAN_POINT('Ctrl Pts',(22.,0.55763177755329,174.999539214703));
#3063=CARTESIAN_POINT('Ctrl Pts',(21.978779974639,1.03421766230349,175.09619314859));
#3064=CARTESIAN_POINT('Ctrl Pts',(21.907804434142,2.14509079920642,175.419604045985));
#3065=CARTESIAN_POINT('Ctrl Pts',(21.8351237457077,2.71999754273336,175.770662232577));
#3066=CARTESIAN_POINT('Ctrl Pts',(21.7231708721587,3.49905157413913,176.393998413372));
#3067=CARTESIAN_POINT('Ctrl Pts',(21.6453341950524,3.95321208636496,176.838841641996));
#3068=CARTESIAN_POINT('Ctrl Pts',(21.5075642574415,4.63936220273143,178.051649859771));
#3069=CARTESIAN_POINT('Ctrl Pts',(21.4569234677635,4.85895980474394,178.684213723796));
#3070=CARTESIAN_POINT('Ctrl Pts',(21.4305680914706,4.97305062459848,179.483986320334));
#3071=CARTESIAN_POINT('Ctrl Pts',(21.4242852856285,4.99999999999998,179.710944260979));
#3072=CARTESIAN_POINT('Ctrl Pts',(21.4242852856285,4.99999999999999,180.));
#3073=CARTESIAN_POINT('',(20.,3.73185018477662E-8,175.000041436213));
#3074=CARTESIAN_POINT('Ctrl Pts',(20.,3.73185018477662E-8,175.000041436213));
#3075=CARTESIAN_POINT('Ctrl Pts',(19.9999999994719,0.283014742405756,174.999786546055));
#3076=CARTESIAN_POINT('Ctrl Pts',(19.9940509156506,0.605923323897178,175.024997930406));
#3077=CARTESIAN_POINT('Ctrl Pts',(19.9609506136869,1.29116251076544,175.161307989225));
#3078=CARTESIAN_POINT('Ctrl Pts',(19.9372461918188,1.61280644746145,175.258019496083));
#3079=CARTESIAN_POINT('Ctrl Pts',(19.8491448581156,2.5265341012254,175.634358550918));
#3080=CARTESIAN_POINT('Ctrl Pts',(19.7675756297683,3.07602021864376,176.001183353682));
#3081=CARTESIAN_POINT('Ctrl Pts',(19.6164573285741,3.91715832709852,176.845369115547));
#3082=CARTESIAN_POINT('Ctrl Pts',(19.5305943144081,4.31837832508637,177.366881965352));
#3083=CARTESIAN_POINT('Ctrl Pts',(19.4157703435753,4.80263665641219,178.554835809988));
#3084=CARTESIAN_POINT('Ctrl Pts',(19.364916731037,5.,179.220409809718));
#3085=CARTESIAN_POINT('Ctrl Pts',(19.364916731037,4.99999999999999,180.));
#3086=CARTESIAN_POINT('Ctrl Pts',(20.,2.19566825658546E-9,184.999950279416));
#3087=CARTESIAN_POINT('Ctrl Pts',(20.0000000000794,-0.723112919238044,185.000675199334));
#3088=CARTESIAN_POINT('Ctrl Pts',(19.9603313151704,-1.33608862318433,184.8382490823));
#3089=CARTESIAN_POINT('Ctrl Pts',(19.861668819025,-2.43933282825348,184.42152350844));
#3090=CARTESIAN_POINT('Ctrl Pts',(19.7812722460709,-2.98500462201654,184.06136107981));
#3091=CARTESIAN_POINT('Ctrl Pts',(19.6467201921559,-3.75669863207033,183.330111124966));
#3092=CARTESIAN_POINT('Ctrl Pts',(19.5535927557505,-4.21754309036747,182.820222354567));
#3093=CARTESIAN_POINT('Ctrl Pts',(19.420273383868,-4.78563378449318,181.518502203014));
#3094=CARTESIAN_POINT('Ctrl Pts',(19.3701649404359,-4.97966702424725,180.883464015848));
#3095=CARTESIAN_POINT('Ctrl Pts',(19.3613269788473,-5.0139081378988,179.497510292478));
#3096=CARTESIAN_POINT('Ctrl Pts',(19.3893990004176,-4.90922242427567,178.866161431178));
#3097=CARTESIAN_POINT('Ctrl Pts',(19.490023993425,-4.49241017983725,177.727574311806));
#3098=CARTESIAN_POINT('Ctrl Pts',(19.5638224334275,-4.17893232584471,177.169356201936));
#3099=CARTESIAN_POINT('Ctrl Pts',(19.7307171512166,-3.30033088115763,176.183284568005));
#3100=CARTESIAN_POINT('Ctrl Pts',(19.8146316030256,-2.77992493069651,175.792923920205));
#3101=CARTESIAN_POINT('Ctrl Pts',(19.9022548761647,-1.98595529578597,175.405568766714));
#3102=CARTESIAN_POINT('Ctrl Pts',(19.9407500804088,-1.61982691968267,175.242872340369));
#3103=CARTESIAN_POINT('Ctrl Pts',(19.9892865959041,-0.749250106435683,175.044322509877));
#3104=CARTESIAN_POINT('Ctrl Pts',(20.000000000697,-0.373578971202775,175.000377890859));
#3105=CARTESIAN_POINT('Ctrl Pts',(20.,3.73179914053834E-8,175.000041436213));
#3106=CARTESIAN_POINT('Origin',(0.,0.,140.));
#3107=CARTESIAN_POINT('',(22.,2.69422295812418E-15,140.));
#3108=CARTESIAN_POINT('Origin',(0.,0.,140.));
#3109=CARTESIAN_POINT('',(20.,2.44929359829471E-15,140.));
#3110=CARTESIAN_POINT('Origin',(0.,0.,140.));
#3111=CARTESIAN_POINT('Origin',(0.,0.,200.));
#3112=CARTESIAN_POINT('',(20.,2.44929359829471E-15,200.));
#3113=CARTESIAN_POINT('',(20.,2.44929359829471E-15,200.));
#3114=CARTESIAN_POINT('',(20.,2.44929359829471E-15,330.));
#3115=CARTESIAN_POINT('',(20.,2.44929359829471E-15,200.));
#3116=CARTESIAN_POINT('Origin',(0.,0.,330.));
#3117=CARTESIAN_POINT('Origin',(0.,0.,200.));
#3118=CARTESIAN_POINT('',(22.,2.69422295812418E-15,330.));
#3119=CARTESIAN_POINT('Origin',(0.,0.,330.));
#3120=CARTESIAN_POINT('',(22.,2.69422295812418E-15,200.));
#3121=CARTESIAN_POINT('',(22.,2.69422295812418E-15,200.));
#3122=CARTESIAN_POINT('',(22.,2.69422295812418E-15,200.));
#3123=CARTESIAN_POINT('Origin',(0.,0.,330.));
#3124=CARTESIAN_POINT('',(0.,0.,0.));
#3125=CARTESIAN_POINT('',(0.,0.,0.));
#3126=CARTESIAN_POINT('',(0.,0.,0.));
#3127=CARTESIAN_POINT('',(0.,0.,0.));
#3128=CARTESIAN_POINT('',(0.,0.,0.));
#3129=CARTESIAN_POINT('',(0.,0.,0.));
#3130=CARTESIAN_POINT('',(0.,0.,0.));
#3131=CARTESIAN_POINT('',(0.,0.,0.));
#3132=CARTESIAN_POINT('',(0.,0.,0.));
#3133=UNCERTAINTY_MEASURE_WITH_UNIT(LENGTH_MEASURE(0.01),#3155,
'DISTANCE_ACCURACY_VALUE',
'Maximum model space distance between geometric entities at asserted c
onnectivities');
#3134=UNCERTAINTY_MEASURE_WITH_UNIT(LENGTH_MEASURE(0.01),#3155,
'DISTANCE_ACCURACY_VALUE',
'Maximum model space distance between geometric entities at asserted c
onnectivities');
#3135=UNCERTAINTY_MEASURE_WITH_UNIT(LENGTH_MEASURE(0.01),#3155,
'DISTANCE_ACCURACY_VALUE',
'Maximum model space distance between geometric entities at asserted c
onnectivities');
#3136=UNCERTAINTY_MEASURE_WITH_UNIT(LENGTH_MEASURE(0.01),#3155,
'DISTANCE_ACCURACY_VALUE',
'Maximum model space distance between geometric entities at asserted c
onnectivities');
#3137=UNCERTAINTY_MEASURE_WITH_UNIT(LENGTH_MEASURE(0.01),#3155,
'DISTANCE_ACCURACY_VALUE',
'Maximum model space distance between geometric entities at asserted c
onnectivities');
#3138=UNCERTAINTY_MEASURE_WITH_UNIT(LENGTH_MEASURE(0.01),#3155,
'DISTANCE_ACCURACY_VALUE',
'Maximum model space distance between geometric entities at asserted c
onnectivities');
#3139=UNCERTAINTY_MEASURE_WITH_UNIT(LENGTH_MEASURE(0.01),#3155,
'DISTANCE_ACCURACY_VALUE',
'Maximum model space distance between geometric entities at asserted c
onnectivities');
#3140=UNCERTAINTY_MEASURE_WITH_UNIT(LENGTH_MEASURE(0.01),#3155,
'DISTANCE_ACCURACY_VALUE',
'Maximum model space distance between geometric entities at asserted c
onnectivities');
#3141=UNCERTAINTY_MEASURE_WITH_UNIT(LENGTH_MEASURE(0.01),#3155,
'DISTANCE_ACCURACY_VALUE',
'Maximum model space distance between geometric entities at asserted c
onnectivities');
#3142=UNCERTAINTY_MEASURE_WITH_UNIT(LENGTH_MEASURE(0.01),#3155,
'DISTANCE_ACCURACY_VALUE',
'Maximum model space distance between geometric entities at asserted c
onnectivities');
#3143=UNCERTAINTY_MEASURE_WITH_UNIT(LENGTH_MEASURE(0.01),#3155,
'DISTANCE_ACCURACY_VALUE',
'Maximum model space distance between geometric entities at asserted c
onnectivities');
#3144=(
GEOMETRIC_REPRESENTATION_CONTEXT(3)
GLOBAL_UNCERTAINTY_ASSIGNED_CONTEXT((#3133))
GLOBAL_UNIT_ASSIGNED_CONTEXT((#3155,#3157,#3158))
REPRESENTATION_CONTEXT('','3D')
);
#3145=(
GEOMETRIC_REPRESENTATION_CONTEXT(3)
GLOBAL_UNCERTAINTY_ASSIGNED_CONTEXT((#3134))
GLOBAL_UNIT_ASSIGNED_CONTEXT((#3155,#3157,#3158))
REPRESENTATION_CONTEXT('','3D')
);
#3146=(
GEOMETRIC_REPRESENTATION_CONTEXT(3)
GLOBAL_UNCERTAINTY_ASSIGNED_CONTEXT((#3135))
GLOBAL_UNIT_ASSIGNED_CONTEXT((#3155,#3157,#3158))
REPRESENTATION_CONTEXT('','3D')
);
#3147=(
GEOMETRIC_REPRESENTATION_CONTEXT(3)
GLOBAL_UNCERTAINTY_ASSIGNED_CONTEXT((#3136))
GLOBAL_UNIT_ASSIGNED_CONTEXT((#3155,#3157,#3158))
REPRESENTATION_CONTEXT('','3D')
);
#3148=(
GEOMETRIC_REPRESENTATION_CONTEXT(3)
GLOBAL_UNCERTAINTY_ASSIGNED_CONTEXT((#3137))
GLOBAL_UNIT_ASSIGNED_CONTEXT((#3155,#3157,#3158))
REPRESENTATION_CONTEXT('','3D')
);
#3149=(
GEOMETRIC_REPRESENTATION_CONTEXT(3)
GLOBAL_UNCERTAINTY_ASSIGNED_CONTEXT((#3138))
GLOBAL_UNIT_ASSIGNED_CONTEXT((#3155,#3157,#3158))
REPRESENTATION_CONTEXT('','3D')
);
#3150=(
GEOMETRIC_REPRESENTATION_CONTEXT(3)
GLOBAL_UNCERTAINTY_ASSIGNED_CONTEXT((#3139))
GLOBAL_UNIT_ASSIGNED_CONTEXT((#3155,#3157,#3158))
REPRESENTATION_CONTEXT('','3D')
);
#3151=(
GEOMETRIC_REPRESENTATION_CONTEXT(3)
GLOBAL_UNCERTAINTY_ASSIGNED_CONTEXT((#3140))
GLOBAL_UNIT_ASSIGNED_CONTEXT((#3155,#3157,#3158))
REPRESENTATION_CONTEXT('','3D')
);
#3152=(
GEOMETRIC_REPRESENTATION_CONTEXT(3)
GLOBAL_UNCERTAINTY_ASSIGNED_CONTEXT((#3141))
GLOBAL_UNIT_ASSIGNED_CONTEXT((#3155,#3157,#3158))
REPRESENTATION_CONTEXT('','3D')
);
#3153=(
GEOMETRIC_REPRESENTATION_CONTEXT(3)
GLOBAL_UNCERTAINTY_ASSIGNED_CONTEXT((#3142))
GLOBAL_UNIT_ASSIGNED_CONTEXT((#3155,#3157,#3158))
REPRESENTATION_CONTEXT('','3D')
);
#3154=(
GEOMETRIC_REPRESENTATION_CONTEXT(3)
GLOBAL_UNCERTAINTY_ASSIGNED_CONTEXT((#3143))
GLOBAL_UNIT_ASSIGNED_CONTEXT((#3155,#3157,#3158))
REPRESENTATION_CONTEXT('','3D')
);
#3155=(
LENGTH_UNIT()
NAMED_UNIT(*)
SI_UNIT(.MILLI.,.METRE.)
);
#3156=(
LENGTH_UNIT()
NAMED_UNIT(*)
SI_UNIT($,.METRE.)
);
#3157=(
NAMED_UNIT(*)
PLANE_ANGLE_UNIT()
SI_UNIT($,.RADIAN.)
);
#3158=(
NAMED_UNIT(*)
SI_UNIT($,.STERADIAN.)
SOLID_ANGLE_UNIT()
);
#3159=SHAPE_DEFINITION_REPRESENTATION(#3169,#3188);
#3160=SHAPE_DEFINITION_REPRESENTATION(#3170,#3189);
#3161=SHAPE_DEFINITION_REPRESENTATION(#3171,#3190);
#3162=SHAPE_DEFINITION_REPRESENTATION(#3172,#3191);
#3163=SHAPE_DEFINITION_REPRESENTATION(#3173,#3192);
#3164=SHAPE_DEFINITION_REPRESENTATION(#3174,#3193);
#3165=SHAPE_DEFINITION_REPRESENTATION(#3175,#3194);
#3166=SHAPE_DEFINITION_REPRESENTATION(#3176,#3195);
#3167=SHAPE_DEFINITION_REPRESENTATION(#3177,#3196);
#3168=SHAPE_DEFINITION_REPRESENTATION(#3178,#3197);
#3169=PRODUCT_DEFINITION_SHAPE('',$,#3199);
#3170=PRODUCT_DEFINITION_SHAPE('',$,#3200);
#3171=PRODUCT_DEFINITION_SHAPE('',$,#3201);
#3172=PRODUCT_DEFINITION_SHAPE('',$,#3202);
#3173=PRODUCT_DEFINITION_SHAPE('',$,#3203);
#3174=PRODUCT_DEFINITION_SHAPE('',$,#3204);
#3175=PRODUCT_DEFINITION_SHAPE('',$,#3205);
#3176=PRODUCT_DEFINITION_SHAPE('',$,#3206);
#3177=PRODUCT_DEFINITION_SHAPE('',$,#3207);
#3178=PRODUCT_DEFINITION_SHAPE('',$,#3208);
#3179=PRODUCT_DEFINITION_SHAPE($,$,#38);
#3180=PRODUCT_DEFINITION_SHAPE($,$,#39);
#3181=PRODUCT_DEFINITION_SHAPE($,$,#40);
#3182=PRODUCT_DEFINITION_SHAPE($,$,#41);
#3183=PRODUCT_DEFINITION_SHAPE($,$,#42);
#3184=PRODUCT_DEFINITION_SHAPE($,$,#43);
#3185=PRODUCT_DEFINITION_SHAPE($,$,#44);
#3186=PRODUCT_DEFINITION_SHAPE($,$,#45);
#3187=PRODUCT_DEFINITION_SHAPE($,$,#46);
#3188=SHAPE_REPRESENTATION('',(#1190,#1277,#1278,#1279,#1280,#1281,#1282,
#1283,#1284,#1285),#3144);
#3189=SHAPE_REPRESENTATION('',(#1191),#3145);
#3190=SHAPE_REPRESENTATION('',(#1202),#3146);
#3191=SHAPE_REPRESENTATION('',(#1212),#3147);
#3192=SHAPE_REPRESENTATION('',(#1221),#3148);
#3193=SHAPE_REPRESENTATION('',(#1230),#3149);
#3194=SHAPE_REPRESENTATION('',(#1239),#3150);
#3195=SHAPE_REPRESENTATION('',(#1248),#3151);
#3196=SHAPE_REPRESENTATION('',(#1257),#3152);
#3197=SHAPE_REPRESENTATION('',(#1266),#3153);
#3198=PRODUCT_DEFINITION_CONTEXT('part definition',#3230,'design');
#3199=PRODUCT_DEFINITION('BR-354','BR-354',#3209,#3198);
#3200=PRODUCT_DEFINITION('Pipe_01','Pipe_01',#3210,#3198);
#3201=PRODUCT_DEFINITION('Cap','Cap',#3211,#3198);
#3202=PRODUCT_DEFINITION('Spring_02','Spring_02',#3212,#3198);
#3203=PRODUCT_DEFINITION('Pine_04','Pine_04',#3213,#3198);
#3204=PRODUCT_DEFINITION('Pine_02','Pine_02',#3214,#3198);
#3205=PRODUCT_DEFINITION('Pine_03','Pine_03',#3215,#3198);
#3206=PRODUCT_DEFINITION('Spring_01','Spring_01',#3216,#3198);
#3207=PRODUCT_DEFINITION('Pine_01','Pine_01',#3217,#3198);
#3208=PRODUCT_DEFINITION('Pipe_02','Pipe_02',#3218,#3198);
#3209=PRODUCT_DEFINITION_FORMATION('',$,#3232);
#3210=PRODUCT_DEFINITION_FORMATION('',$,#3233);
#3211=PRODUCT_DEFINITION_FORMATION('',$,#3234);
#3212=PRODUCT_DEFINITION_FORMATION('',$,#3235);
#3213=PRODUCT_DEFINITION_FORMATION('',$,#3236);
#3214=PRODUCT_DEFINITION_FORMATION('',$,#3237);
#3215=PRODUCT_DEFINITION_FORMATION('',$,#3238);
#3216=PRODUCT_DEFINITION_FORMATION('',$,#3239);
#3217=PRODUCT_DEFINITION_FORMATION('',$,#3240);
#3218=PRODUCT_DEFINITION_FORMATION('',$,#3241);
#3219=PRODUCT_RELATED_PRODUCT_CATEGORY('BR-354','BR-354',(#3232));
#3220=PRODUCT_RELATED_PRODUCT_CATEGORY('Pipe_01','Pipe_01',(#3233));
#3221=PRODUCT_RELATED_PRODUCT_CATEGORY('Cap','Cap',(#3234));
#3222=PRODUCT_RELATED_PRODUCT_CATEGORY('Spring_02','Spring_02',(#3235));
#3223=PRODUCT_RELATED_PRODUCT_CATEGORY('Pine_04','Pine_04',(#3236));
#3224=PRODUCT_RELATED_PRODUCT_CATEGORY('Pine_02','Pine_02',(#3237));
#3225=PRODUCT_RELATED_PRODUCT_CATEGORY('Pine_03','Pine_03',(#3238));
#3226=PRODUCT_RELATED_PRODUCT_CATEGORY('Spring_01','Spring_01',(#3239));
#3227=PRODUCT_RELATED_PRODUCT_CATEGORY('Pine_01','Pine_01',(#3240));
#3228=PRODUCT_RELATED_PRODUCT_CATEGORY('Pipe_02','Pipe_02',(#3241));
#3229=APPLICATION_PROTOCOL_DEFINITION('international standard',
'automotive_design',2009,#3230);
#3230=APPLICATION_CONTEXT(
'Core Data for Automotive Mechanical Design Process');
#3231=PRODUCT_CONTEXT('part definition',#3230,'mechanical');
#3232=PRODUCT('BR-354','BR-354',$,(#3231));
#3233=PRODUCT('Pipe_01','Pipe_01',$,(#3231));
#3234=PRODUCT('Cap','Cap',$,(#3231));
#3235=PRODUCT('Spring_02','Spring_02',$,(#3231));
#3236=PRODUCT('Pine_04','Pine_04',$,(#3231));
#3237=PRODUCT('Pine_02','Pine_02',$,(#3231));
#3238=PRODUCT('Pine_03','Pine_03',$,(#3231));
#3239=PRODUCT('Spring_01','Spring_01',$,(#3231));
#3240=PRODUCT('Pine_01','Pine_01',$,(#3231));
#3241=PRODUCT('Pipe_02','Pipe_02',$,(#3231));
#3242=PRESENTATION_STYLE_ASSIGNMENT((#3244));
#3243=PRESENTATION_STYLE_ASSIGNMENT((#3245));
#3244=SURFACE_STYLE_USAGE(.BOTH.,#3246);
#3245=SURFACE_STYLE_USAGE(.BOTH.,#3247);
#3246=SURFACE_SIDE_STYLE('',(#3248));
#3247=SURFACE_SIDE_STYLE('',(#3249));
#3248=SURFACE_STYLE_FILL_AREA(#3250);
#3249=SURFACE_STYLE_FILL_AREA(#3251);
#3250=FILL_AREA_STYLE('Steel - Satin',(#3252));
#3251=FILL_AREA_STYLE('Opaque(160,160,160)',(#3253));
#3252=FILL_AREA_STYLE_COLOUR('Steel - Satin',#3254);
#3253=FILL_AREA_STYLE_COLOUR('Opaque(160,160,160)',#3255);
#3254=COLOUR_RGB('Steel - Satin', 0.09019608, 0.27058824, 0.51372549);
#3255=COLOUR_RGB('Opaque(160,160,160)', 0.09019608, 0.27058824, 0.51372549);
ENDSEC;
END-ISO-10303-21;
